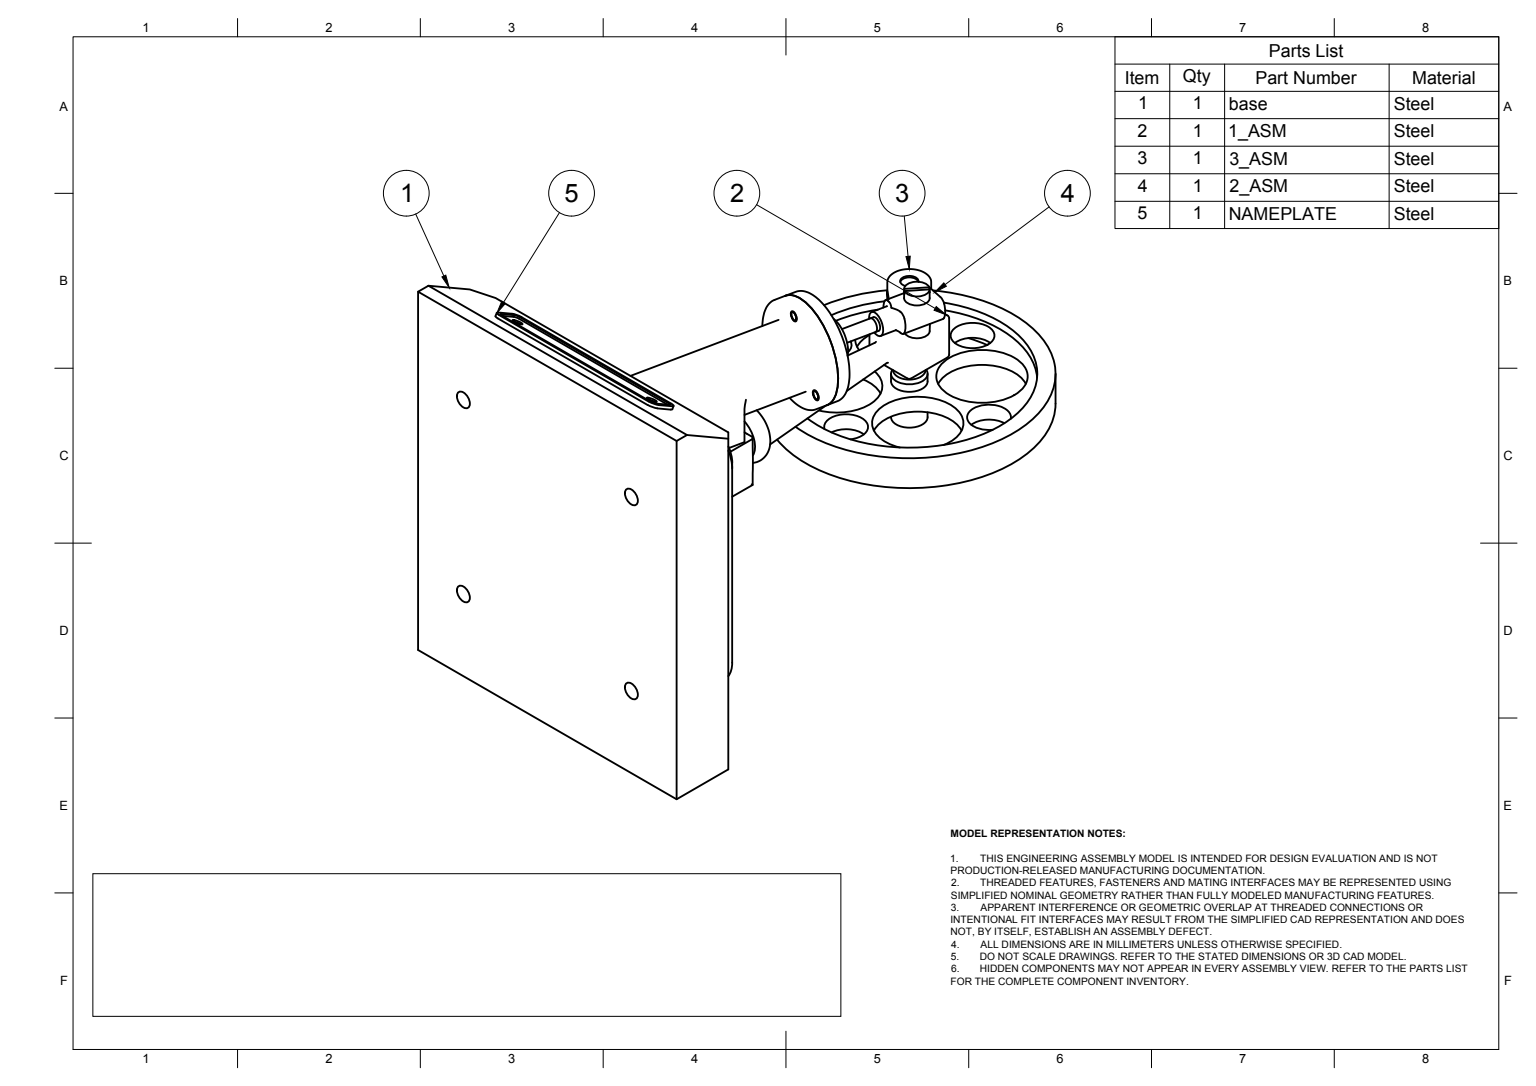
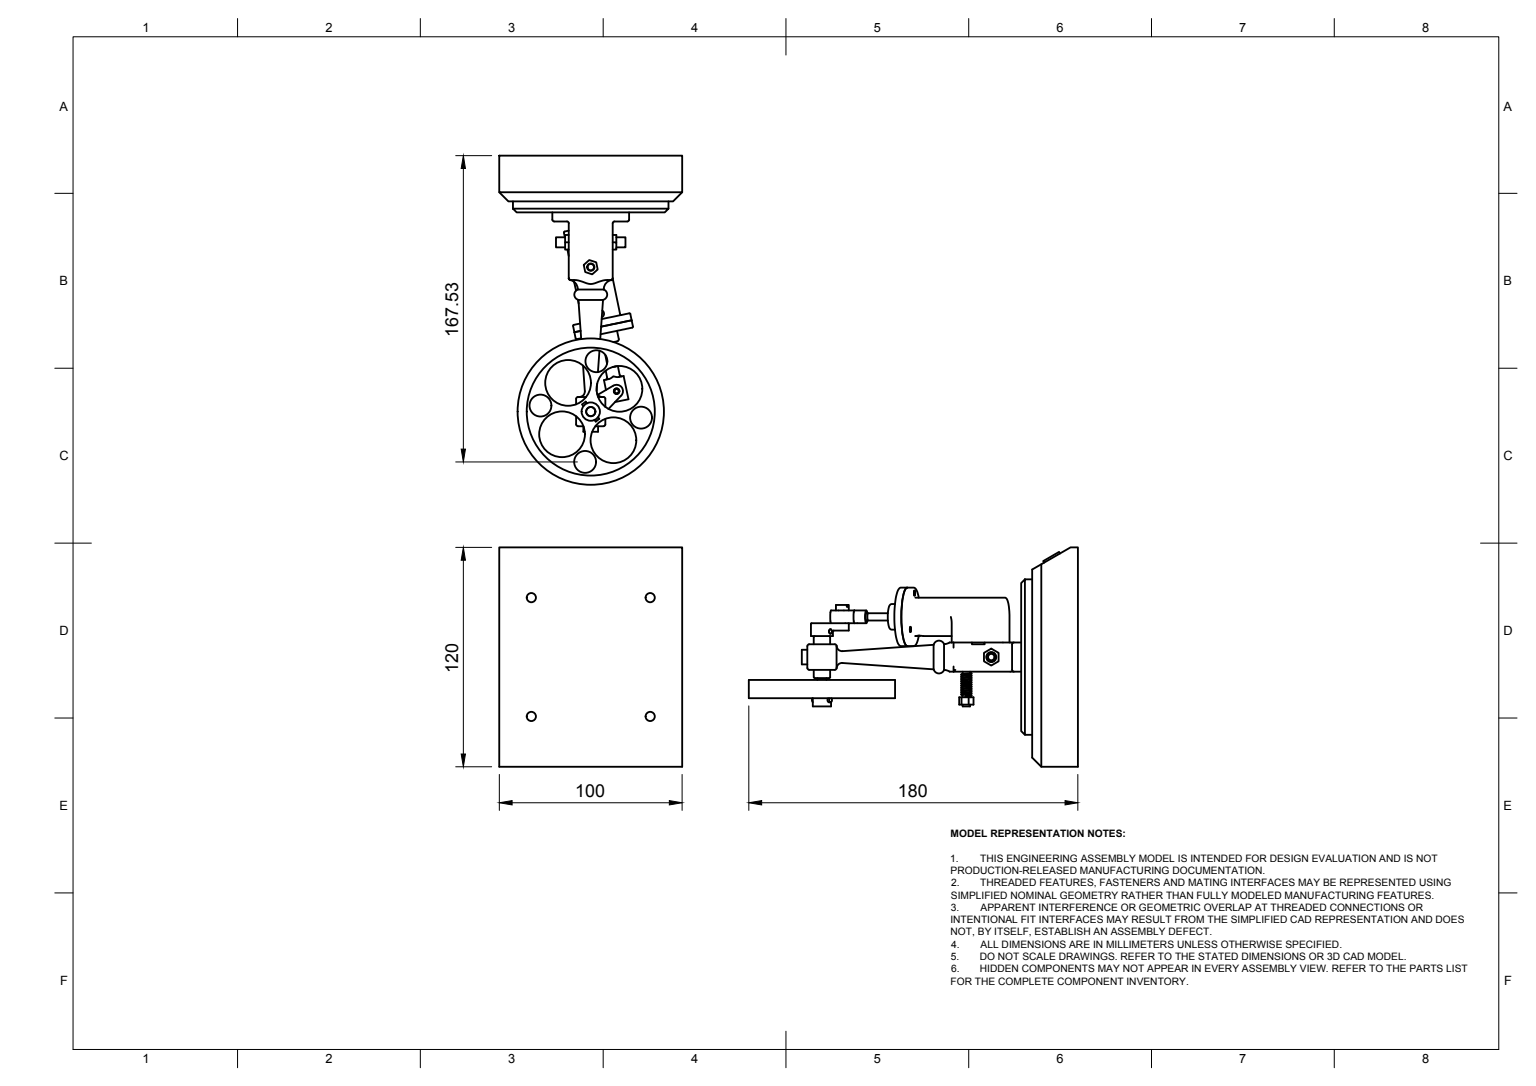
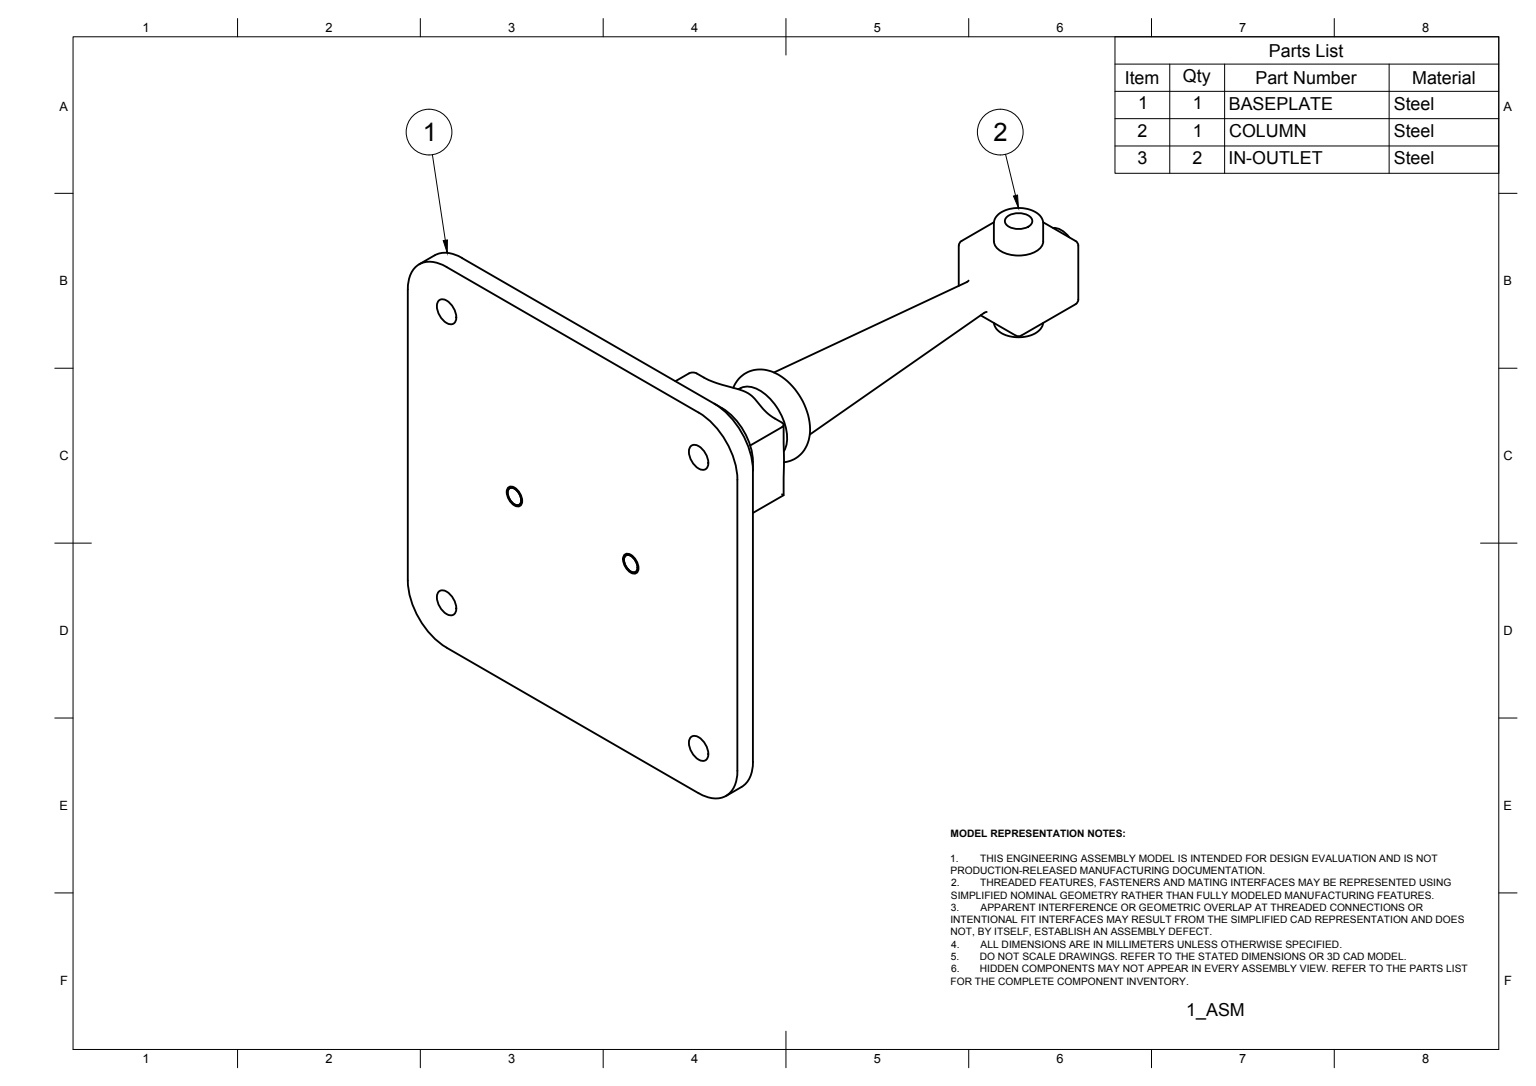
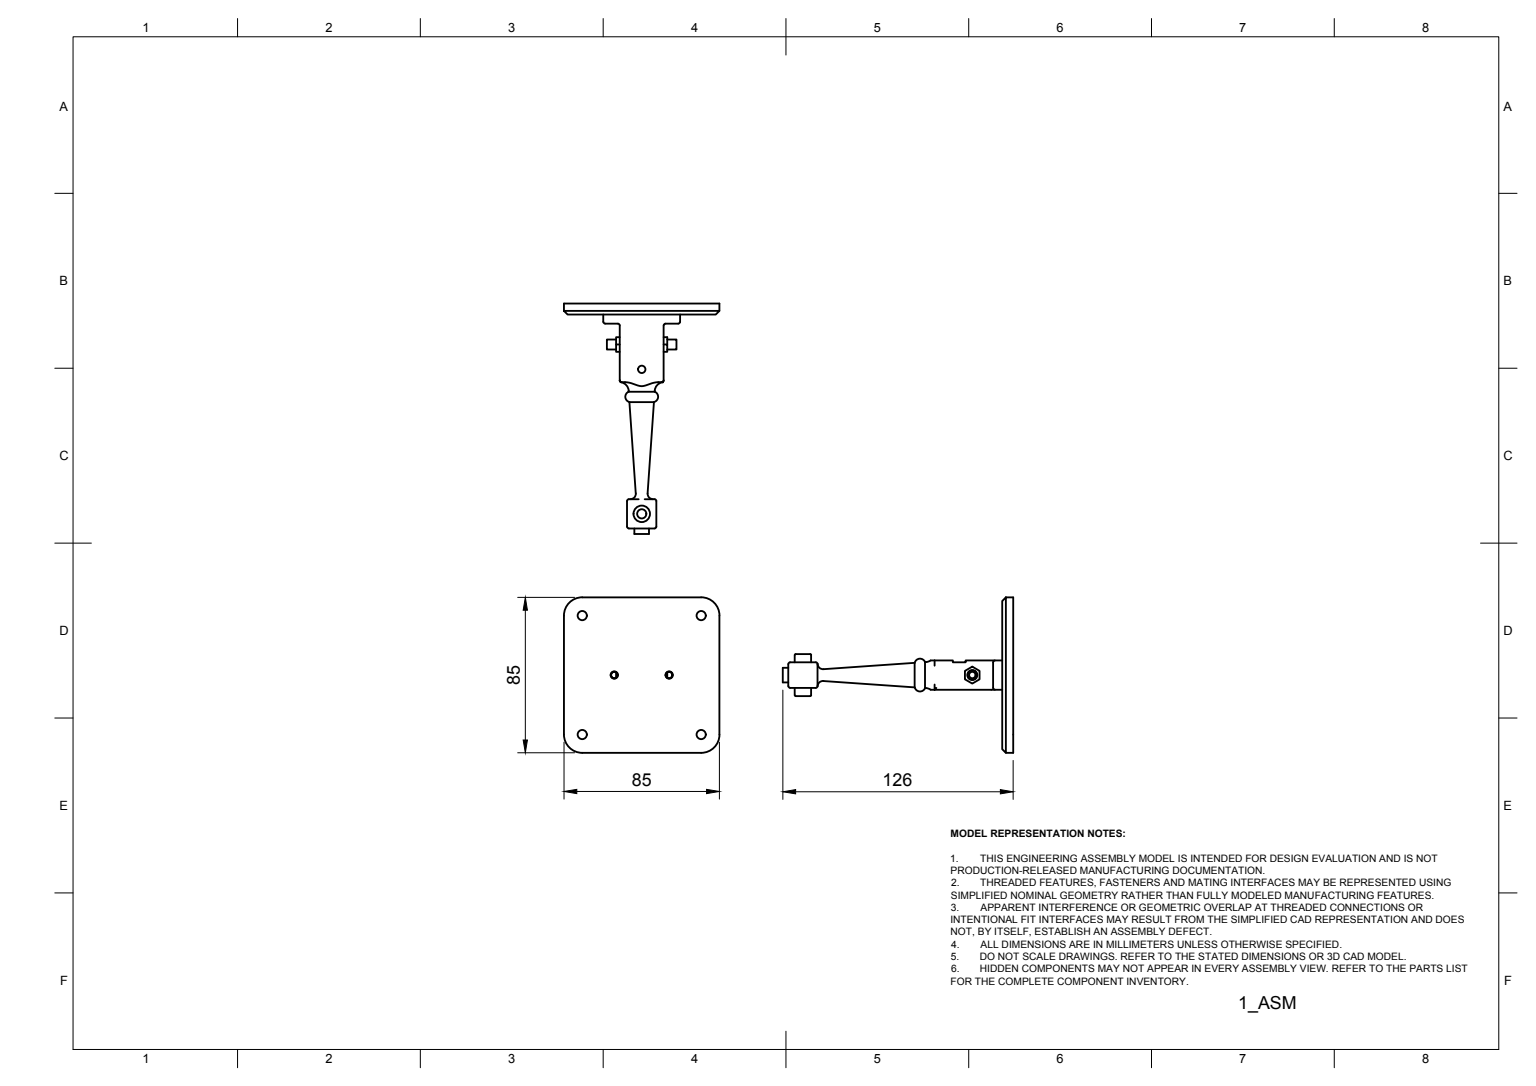
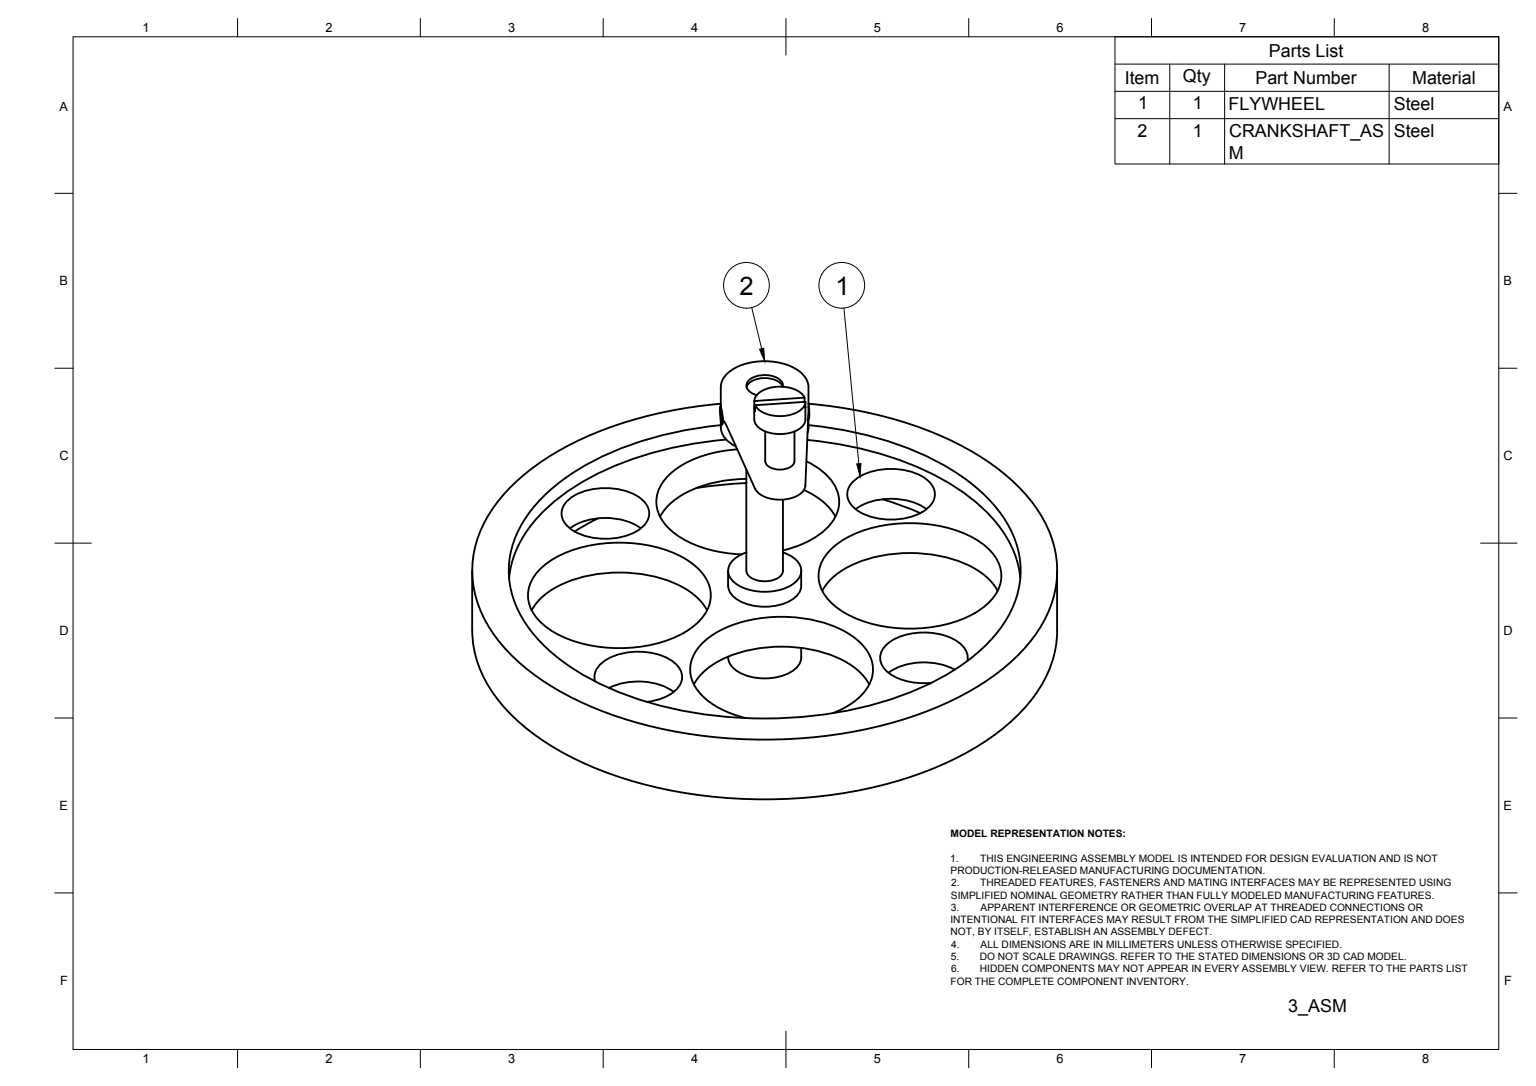
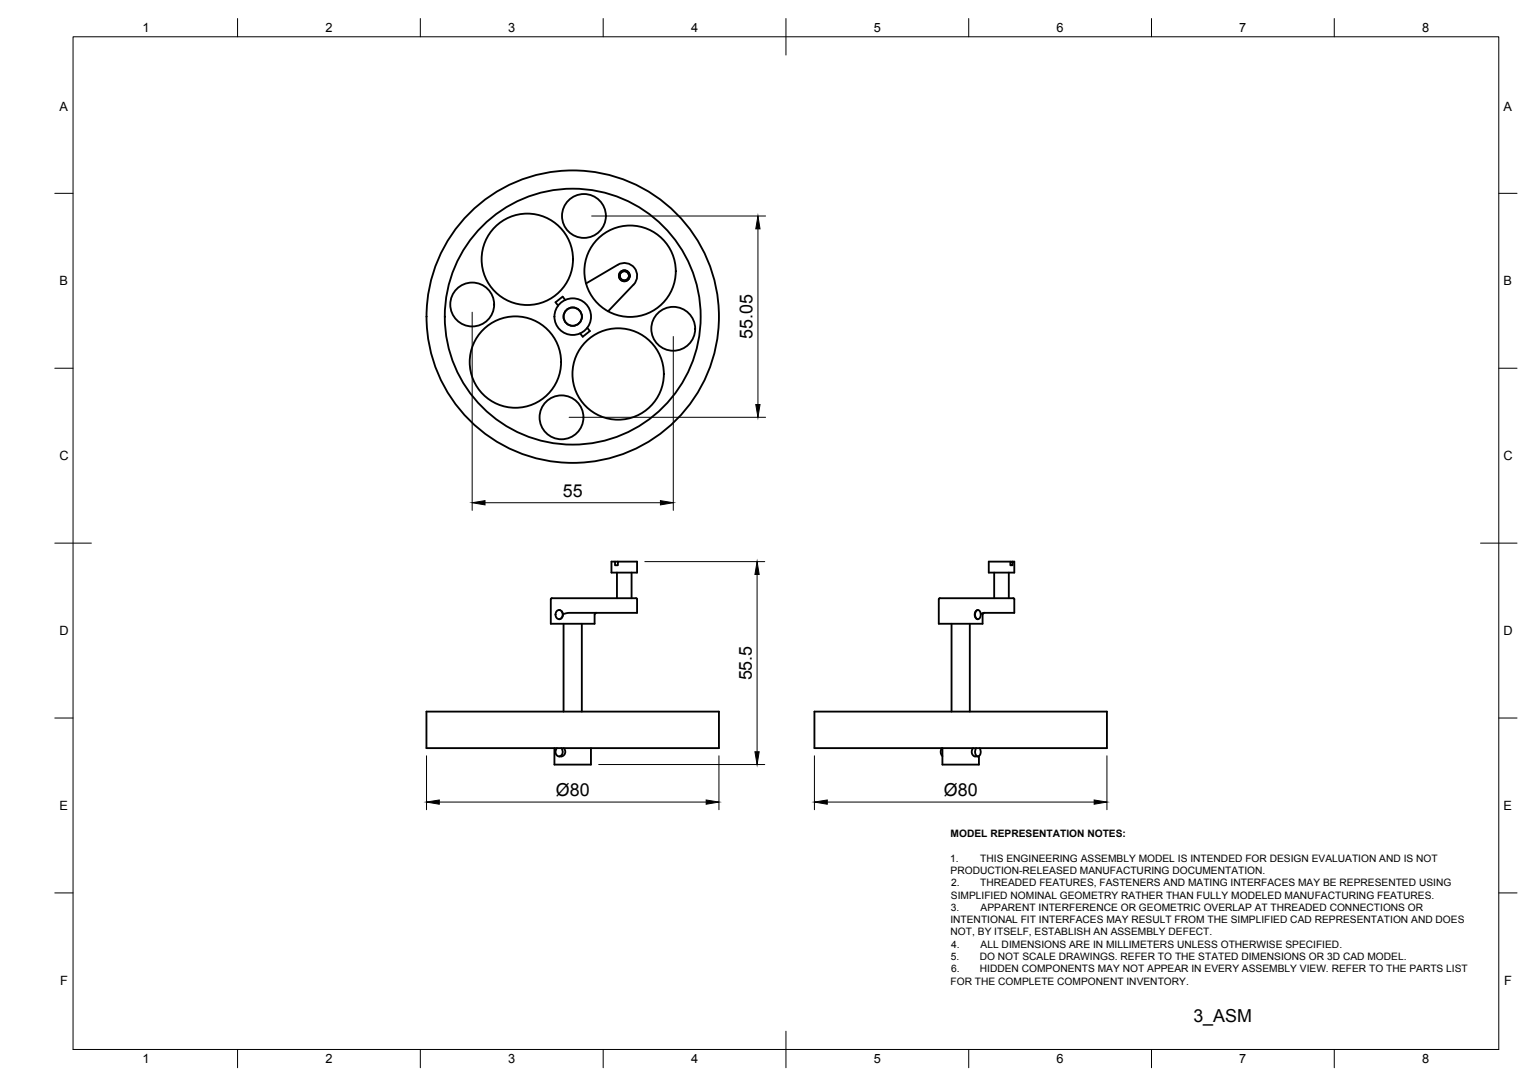
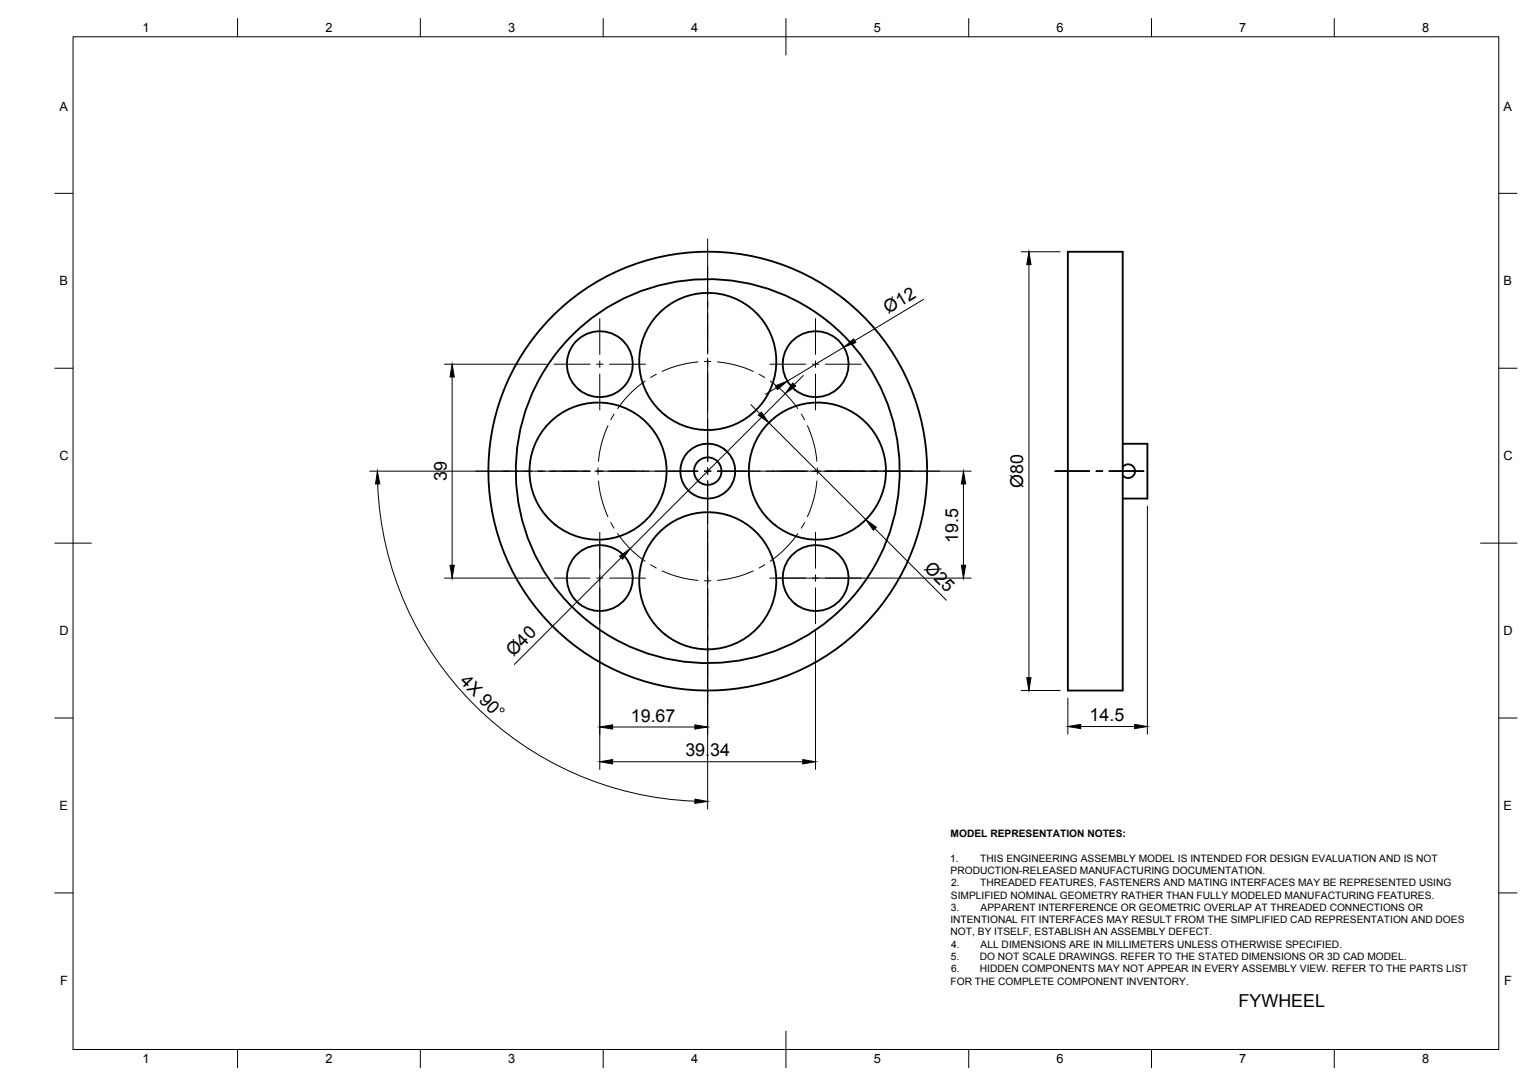
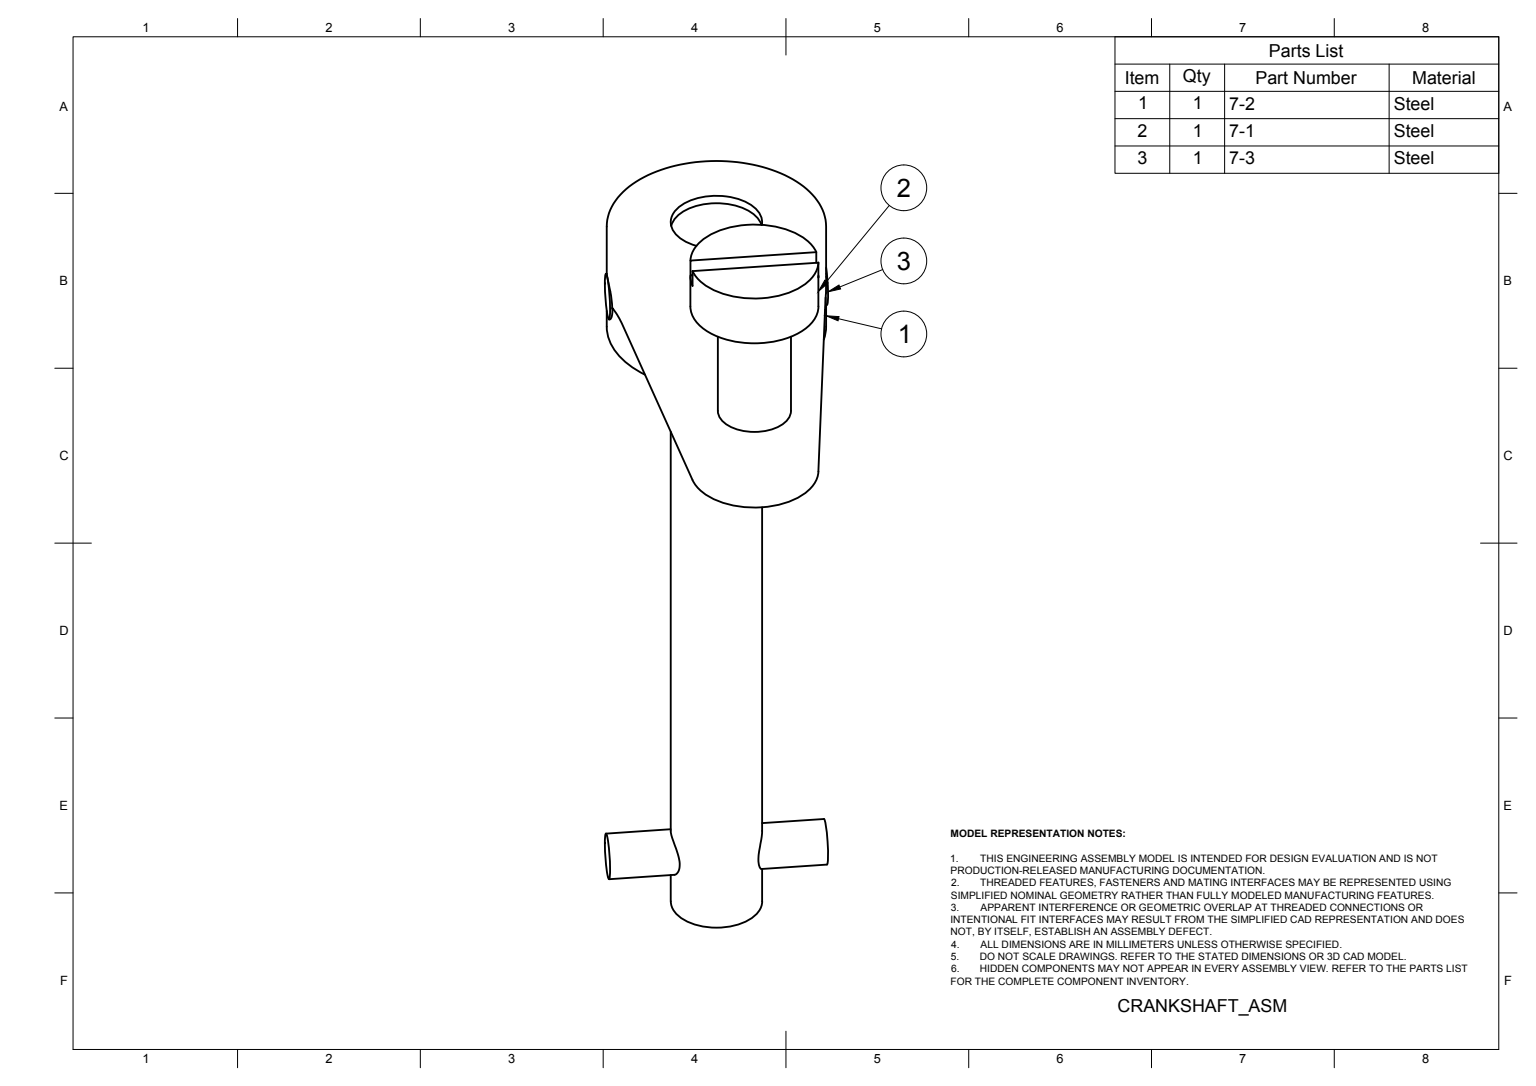
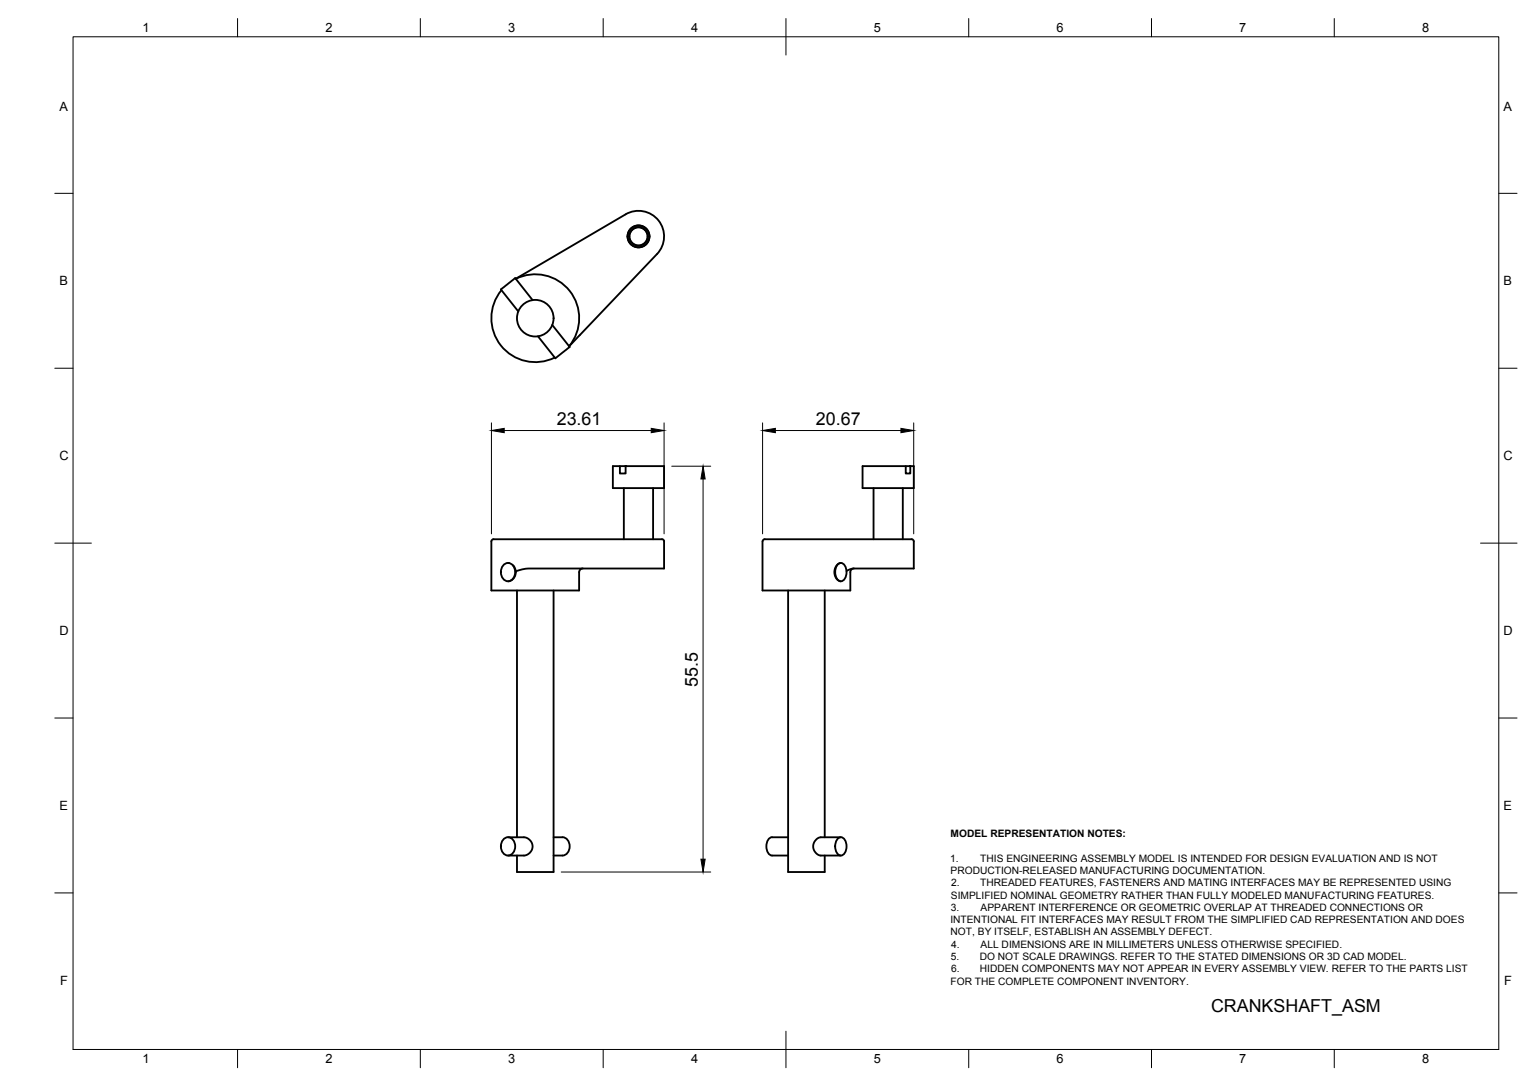
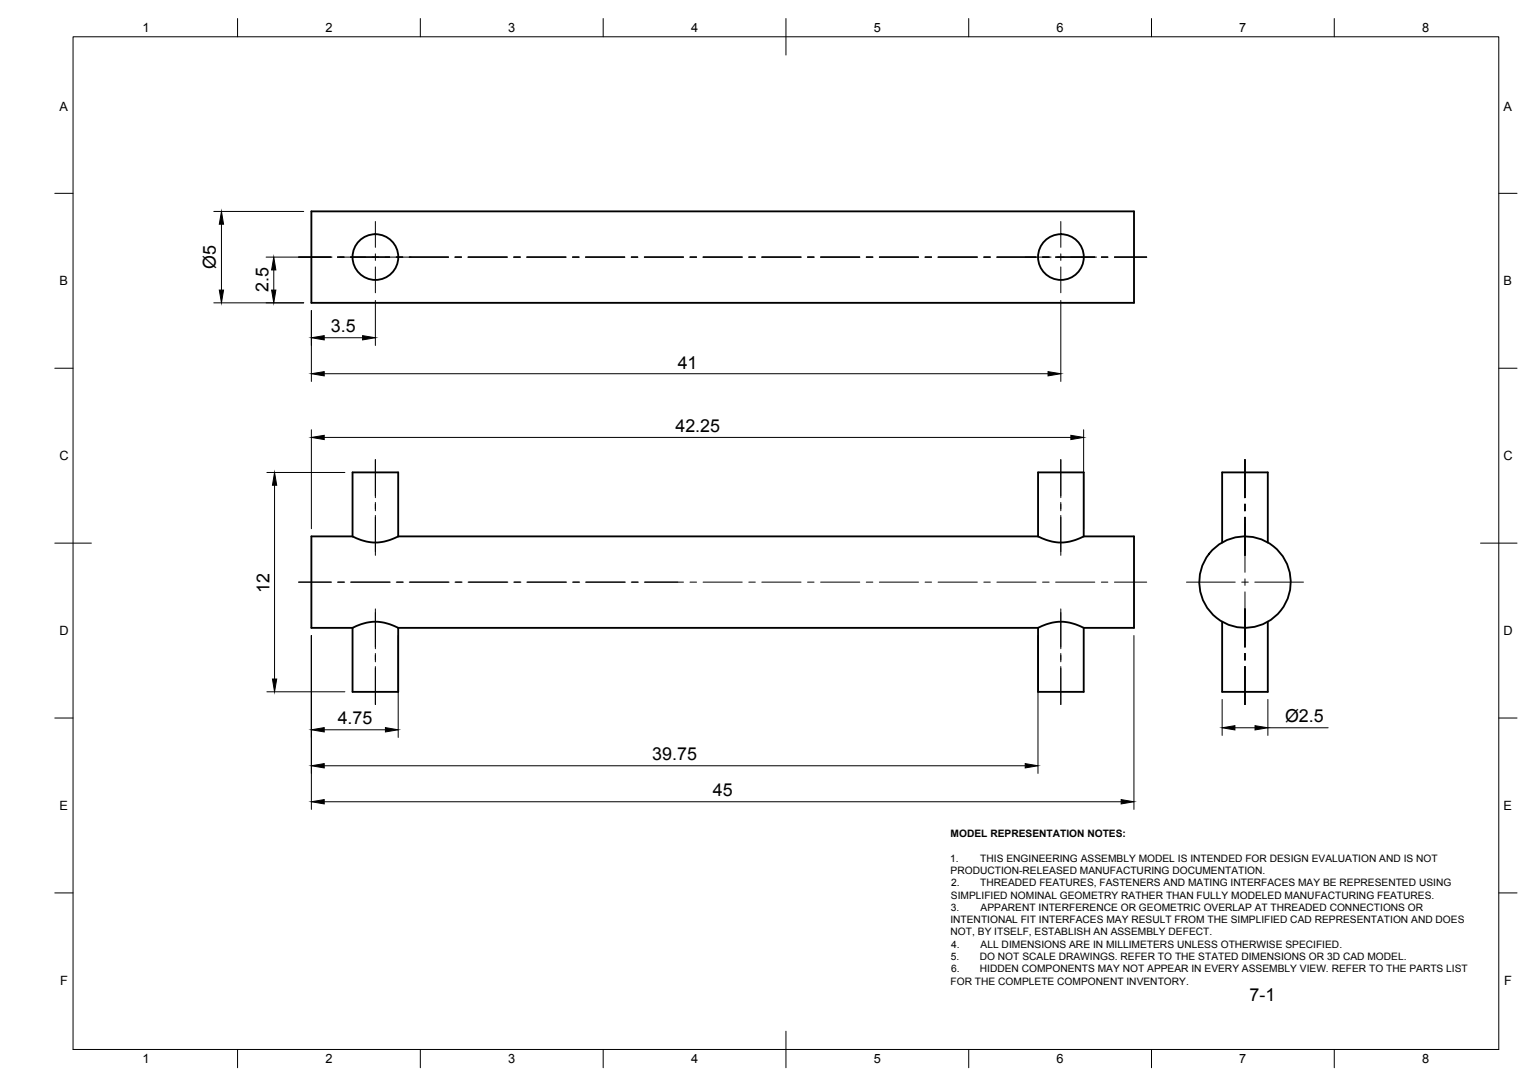
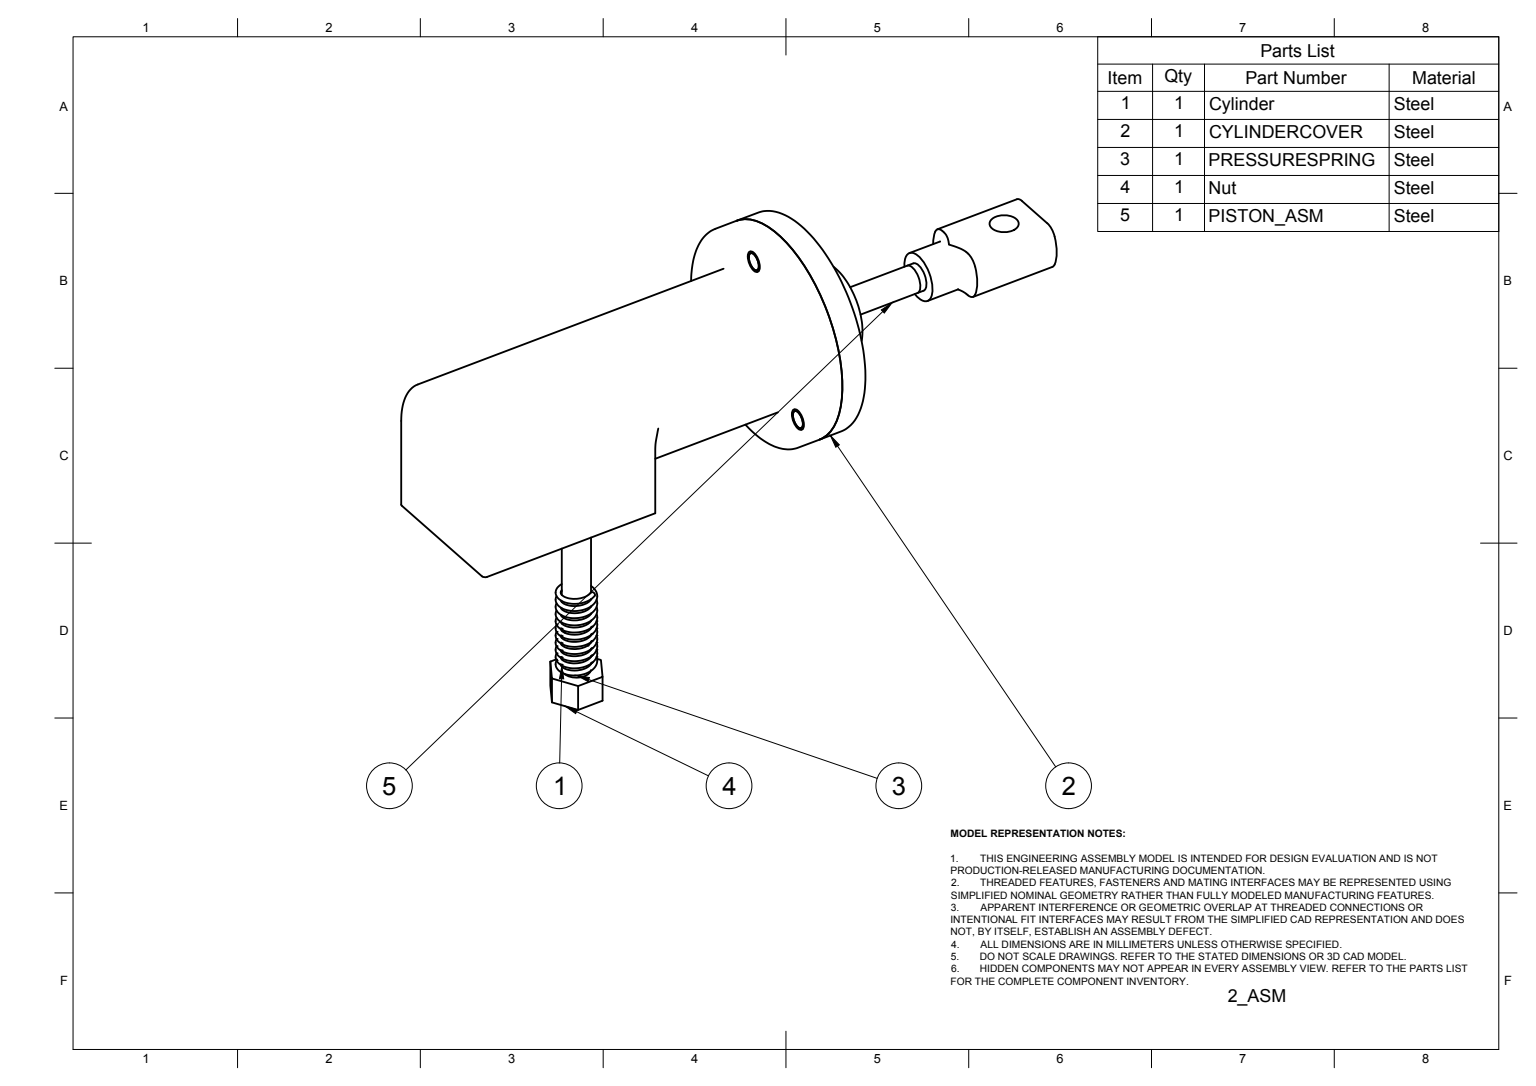
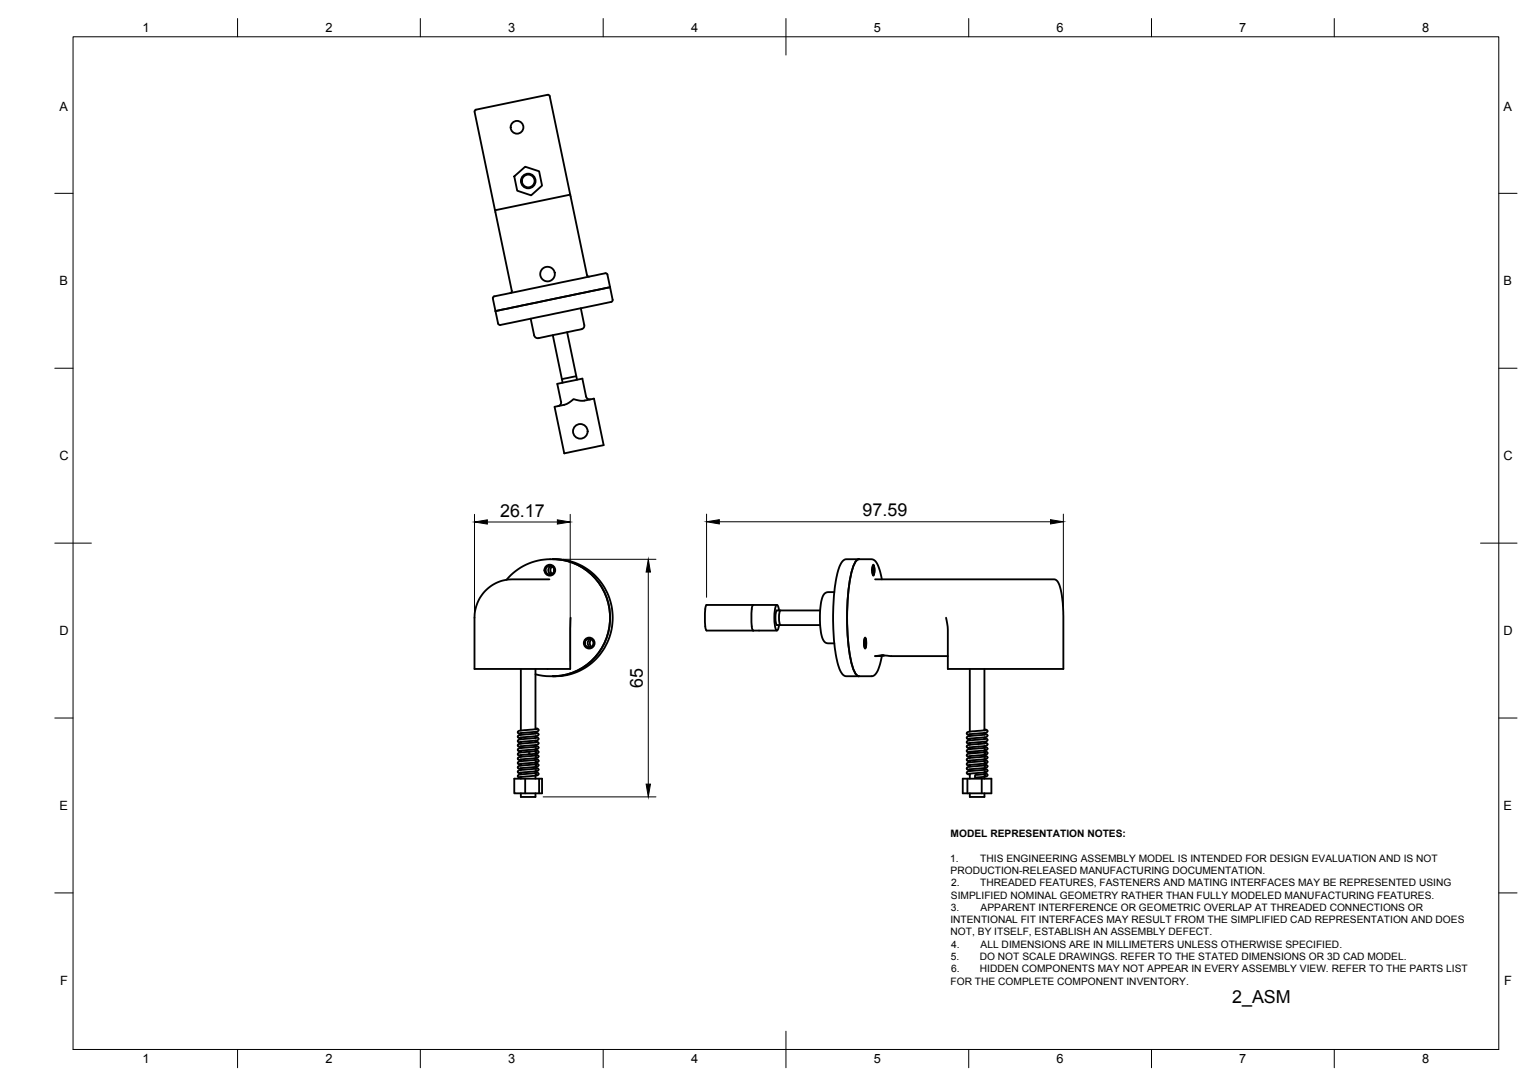
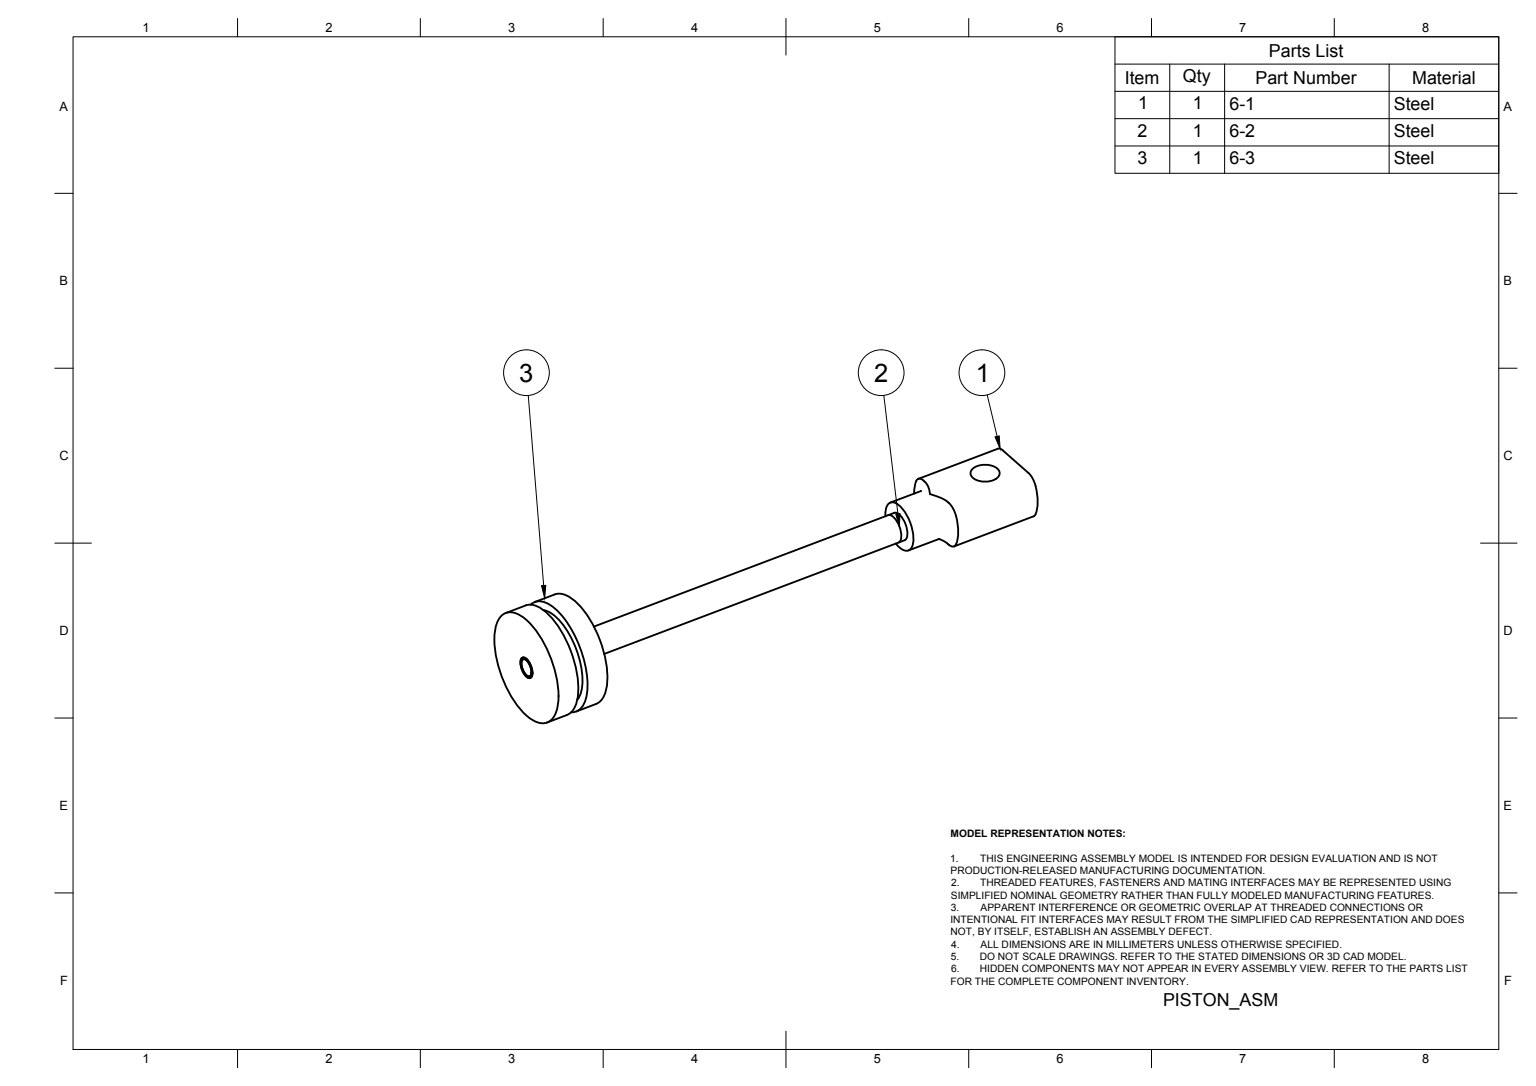
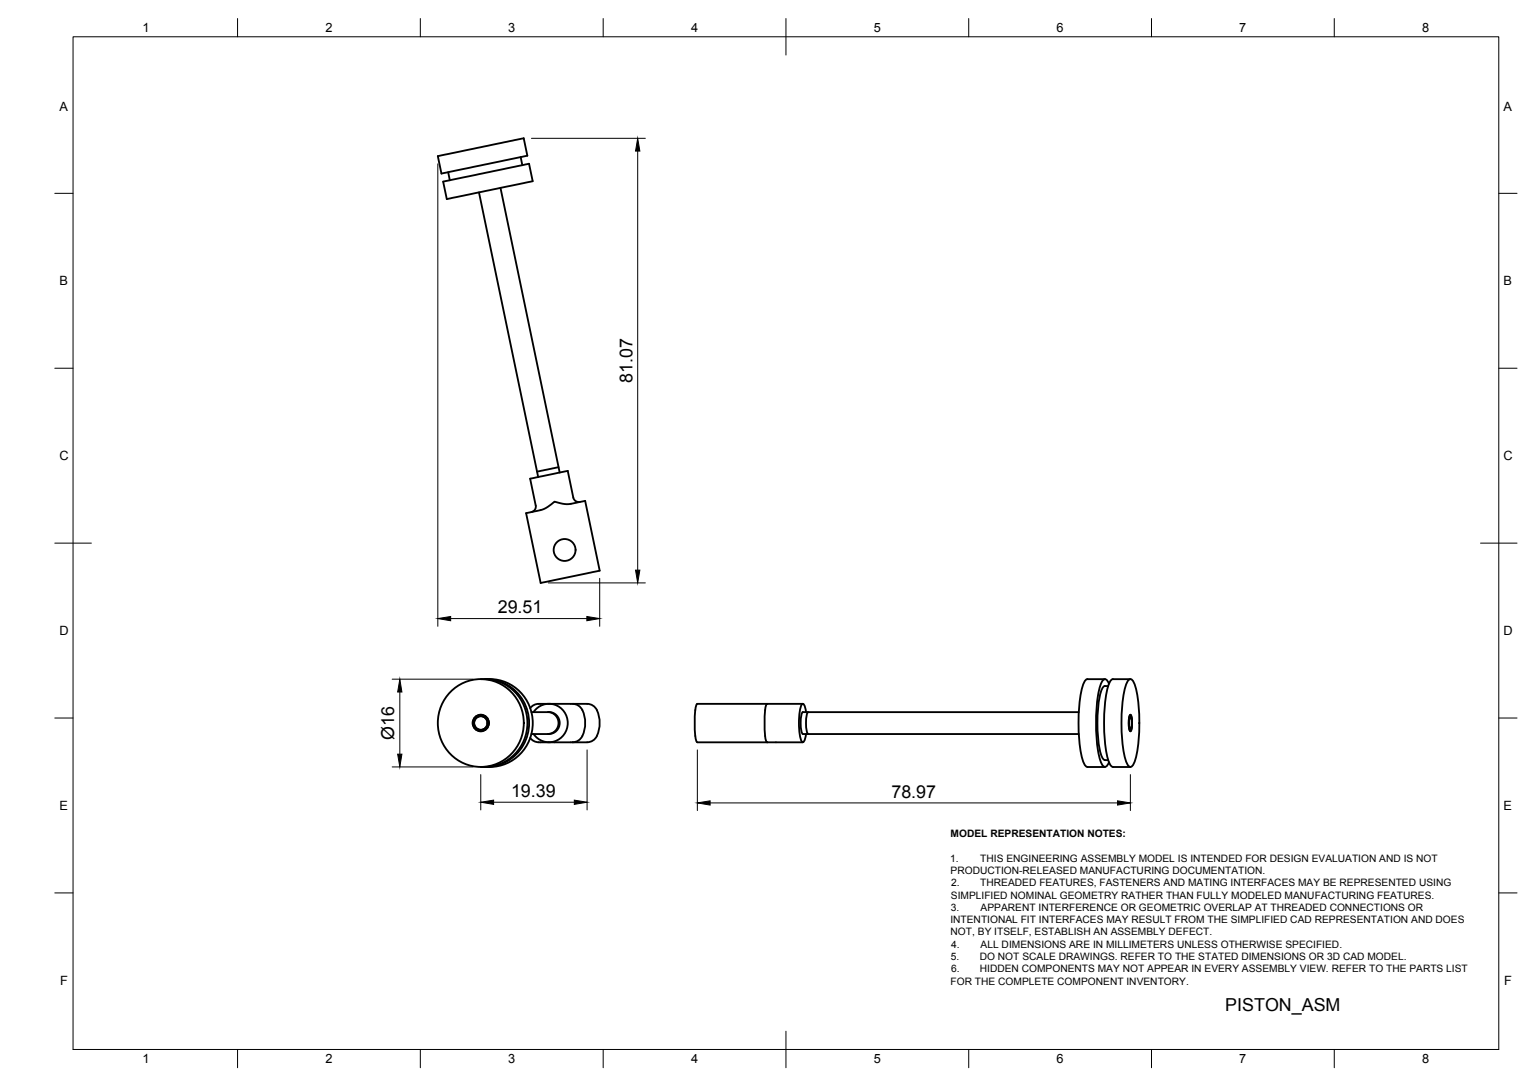
ISO-10303-21;
HEADER;
/* Generated by software containing ST-Developer
 * from STEP Tools, Inc. (www.steptools.com) 
 */

FILE_DESCRIPTION(
/* description */ (''),
/* implementation_level */ '2;1');

FILE_NAME(
/* name */ 'MAS-613',
/* time_stamp */ '2026-10-06T01:16:10-07:00',
/* author */ (''),
/* organization */ (''),
/* preprocessor_version */ 'ST-DEVELOPER v20.2',
/* originating_system */ 'Autodesk Translation Framework v15.15.0.0',
/* authorisation */ '');

FILE_SCHEMA (('AUTOMOTIVE_DESIGN { 1 0 10303 214 3 1 1 }'));
ENDSEC;

DATA;
#10=MECHANICAL_DESIGN_GEOMETRIC_PRESENTATION_REPRESENTATION('',(#296,#297,
#298,#299,#300,#301,#302,#303,#304,#305,#306,#307,#308,#309,#310,#311,#312,
#313,#314,#315,#316,#317,#318,#319,#320,#321,#322,#323,#324,#325,#326,#327,
#328,#329),#17113);
#11=B_SPLINE_SURFACE_WITH_KNOTS('',3,3,((#11570,#11571,#11572,#11573,#11574,
#11575,#11576,#11577,#11578,#11579,#11580,#11581,#11582,#11583,#11584,#11585,
#11586,#11587,#11588,#11589,#11590,#11591,#11592,#11593,#11594,#11595,#11596,
#11597,#11598,#11599,#11600,#11601,#11602,#11603,#11604),(#11605,#11606,
#11607,#11608,#11609,#11610,#11611,#11612,#11613,#11614,#11615,#11616,#11617,
#11618,#11619,#11620,#11621,#11622,#11623,#11624,#11625,#11626,#11627,#11628,
#11629,#11630,#11631,#11632,#11633,#11634,#11635,#11636,#11637,#11638,#11639),
(#11640,#11641,#11642,#11643,#11644,#11645,#11646,#11647,#11648,#11649,
#11650,#11651,#11652,#11653,#11654,#11655,#11656,#11657,#11658,#11659,#11660,
#11661,#11662,#11663,#11664,#11665,#11666,#11667,#11668,#11669,#11670,#11671,
#11672,#11673,#11674),(#11675,#11676,#11677,#11678,#11679,#11680,#11681,
#11682,#11683,#11684,#11685,#11686,#11687,#11688,#11689,#11690,#11691,#11692,
#11693,#11694,#11695,#11696,#11697,#11698,#11699,#11700,#11701,#11702,#11703,
#11704,#11705,#11706,#11707,#11708,#11709),(#11710,#11711,#11712,#11713,
#11714,#11715,#11716,#11717,#11718,#11719,#11720,#11721,#11722,#11723,#11724,
#11725,#11726,#11727,#11728,#11729,#11730,#11731,#11732,#11733,#11734,#11735,
#11736,#11737,#11738,#11739,#11740,#11741,#11742,#11743,#11744),(#11745,
#11746,#11747,#11748,#11749,#11750,#11751,#11752,#11753,#11754,#11755,#11756,
#11757,#11758,#11759,#11760,#11761,#11762,#11763,#11764,#11765,#11766,#11767,
#11768,#11769,#11770,#11771,#11772,#11773,#11774,#11775,#11776,#11777,#11778,
#11779),(#11780,#11781,#11782,#11783,#11784,#11785,#11786,#11787,#11788,
#11789,#11790,#11791,#11792,#11793,#11794,#11795,#11796,#11797,#11798,#11799,
#11800,#11801,#11802,#11803,#11804,#11805,#11806,#11807,#11808,#11809,#11810,
#11811,#11812,#11813,#11814),(#11815,#11816,#11817,#11818,#11819,#11820,
#11821,#11822,#11823,#11824,#11825,#11826,#11827,#11828,#11829,#11830,#11831,
#11832,#11833,#11834,#11835,#11836,#11837,#11838,#11839,#11840,#11841,#11842,
#11843,#11844,#11845,#11846,#11847,#11848,#11849),(#11850,#11851,#11852,
#11853,#11854,#11855,#11856,#11857,#11858,#11859,#11860,#11861,#11862,#11863,
#11864,#11865,#11866,#11867,#11868,#11869,#11870,#11871,#11872,#11873,#11874,
#11875,#11876,#11877,#11878,#11879,#11880,#11881,#11882,#11883,#11884),
(#11885,#11886,#11887,#11888,#11889,#11890,#11891,#11892,#11893,#11894,
#11895,#11896,#11897,#11898,#11899,#11900,#11901,#11902,#11903,#11904,#11905,
#11906,#11907,#11908,#11909,#11910,#11911,#11912,#11913,#11914,#11915,#11916,
#11917,#11918,#11919)),.UNSPECIFIED.,.F.,.F.,.F.,(4,1,1,1,1,1,1,4),(4,1,
1,1,1,1,1,1,1,1,1,1,1,1,1,1,1,1,1,1,1,1,1,1,1,1,1,1,1,1,1,1,4),(-0.05714514294858,
0.,0.125,0.25,0.3267862857371,0.4035725714743,0.4803588572114,0.5571451429486),
(-0.02,0.0125,0.045,0.0775,0.11,0.1425,0.175,0.2075,0.24,0.2725,0.305,0.3375,
0.37,0.4025,0.435,0.4675,0.5,0.5325,0.565,0.5975,0.63,0.6625,0.695,0.7275,
0.76,0.7925,0.825,0.8575,0.89,0.9225,0.955,0.9875,1.02),.UNSPECIFIED.);
#12=B_SPLINE_SURFACE_WITH_KNOTS('',3,3,((#13047,#13048,#13049,#13050,#13051,
#13052,#13053,#13054,#13055,#13056,#13057,#13058,#13059,#13060,#13061,#13062,
#13063,#13064,#13065,#13066,#13067,#13068,#13069,#13070,#13071,#13072,#13073,
#13074,#13075,#13076,#13077,#13078,#13079,#13080,#13081),(#13082,#13083,
#13084,#13085,#13086,#13087,#13088,#13089,#13090,#13091,#13092,#13093,#13094,
#13095,#13096,#13097,#13098,#13099,#13100,#13101,#13102,#13103,#13104,#13105,
#13106,#13107,#13108,#13109,#13110,#13111,#13112,#13113,#13114,#13115,#13116),
(#13117,#13118,#13119,#13120,#13121,#13122,#13123,#13124,#13125,#13126,
#13127,#13128,#13129,#13130,#13131,#13132,#13133,#13134,#13135,#13136,#13137,
#13138,#13139,#13140,#13141,#13142,#13143,#13144,#13145,#13146,#13147,#13148,
#13149,#13150,#13151),(#13152,#13153,#13154,#13155,#13156,#13157,#13158,
#13159,#13160,#13161,#13162,#13163,#13164,#13165,#13166,#13167,#13168,#13169,
#13170,#13171,#13172,#13173,#13174,#13175,#13176,#13177,#13178,#13179,#13180,
#13181,#13182,#13183,#13184,#13185,#13186),(#13187,#13188,#13189,#13190,
#13191,#13192,#13193,#13194,#13195,#13196,#13197,#13198,#13199,#13200,#13201,
#13202,#13203,#13204,#13205,#13206,#13207,#13208,#13209,#13210,#13211,#13212,
#13213,#13214,#13215,#13216,#13217,#13218,#13219,#13220,#13221),(#13222,
#13223,#13224,#13225,#13226,#13227,#13228,#13229,#13230,#13231,#13232,#13233,
#13234,#13235,#13236,#13237,#13238,#13239,#13240,#13241,#13242,#13243,#13244,
#13245,#13246,#13247,#13248,#13249,#13250,#13251,#13252,#13253,#13254,#13255,
#13256),(#13257,#13258,#13259,#13260,#13261,#13262,#13263,#13264,#13265,
#13266,#13267,#13268,#13269,#13270,#13271,#13272,#13273,#13274,#13275,#13276,
#13277,#13278,#13279,#13280,#13281,#13282,#13283,#13284,#13285,#13286,#13287,
#13288,#13289,#13290,#13291)),.UNSPECIFIED.,.F.,.F.,.F.,(4,1,1,1,4),(4,
1,1,1,1,1,1,1,1,1,1,1,1,1,1,1,1,1,1,1,1,1,1,1,1,1,1,1,1,1,1,1,4),(0.4428548570514,
0.5,0.75,1.,1.057145142949),(-0.02,0.0125,0.045,0.0775,0.11,0.1425,0.175,
0.2075,0.24,0.2725,0.305,0.3375,0.37,0.4025,0.435,0.4675,0.5,0.5325,0.565,
0.5975,0.63,0.6625,0.695,0.7275,0.76,0.7925,0.825,0.8575,0.89,0.9225,0.955,
0.9875,1.02),.UNSPECIFIED.);
#13=B_SPLINE_SURFACE_WITH_KNOTS('',3,3,((#13335,#13336,#13337,#13338,#13339,
#13340,#13341,#13342,#13343,#13344,#13345,#13346,#13347,#13348,#13349,#13350,
#13351,#13352,#13353,#13354,#13355,#13356,#13357,#13358,#13359,#13360,#13361,
#13362,#13363,#13364,#13365,#13366,#13367,#13368,#13369),(#13370,#13371,
#13372,#13373,#13374,#13375,#13376,#13377,#13378,#13379,#13380,#13381,#13382,
#13383,#13384,#13385,#13386,#13387,#13388,#13389,#13390,#13391,#13392,#13393,
#13394,#13395,#13396,#13397,#13398,#13399,#13400,#13401,#13402,#13403,#13404),
(#13405,#13406,#13407,#13408,#13409,#13410,#13411,#13412,#13413,#13414,
#13415,#13416,#13417,#13418,#13419,#13420,#13421,#13422,#13423,#13424,#13425,
#13426,#13427,#13428,#13429,#13430,#13431,#13432,#13433,#13434,#13435,#13436,
#13437,#13438,#13439),(#13440,#13441,#13442,#13443,#13444,#13445,#13446,
#13447,#13448,#13449,#13450,#13451,#13452,#13453,#13454,#13455,#13456,#13457,
#13458,#13459,#13460,#13461,#13462,#13463,#13464,#13465,#13466,#13467,#13468,
#13469,#13470,#13471,#13472,#13473,#13474),(#13475,#13476,#13477,#13478,
#13479,#13480,#13481,#13482,#13483,#13484,#13485,#13486,#13487,#13488,#13489,
#13490,#13491,#13492,#13493,#13494,#13495,#13496,#13497,#13498,#13499,#13500,
#13501,#13502,#13503,#13504,#13505,#13506,#13507,#13508,#13509),(#13510,
#13511,#13512,#13513,#13514,#13515,#13516,#13517,#13518,#13519,#13520,#13521,
#13522,#13523,#13524,#13525,#13526,#13527,#13528,#13529,#13530,#13531,#13532,
#13533,#13534,#13535,#13536,#13537,#13538,#13539,#13540,#13541,#13542,#13543,
#13544),(#13545,#13546,#13547,#13548,#13549,#13550,#13551,#13552,#13553,
#13554,#13555,#13556,#13557,#13558,#13559,#13560,#13561,#13562,#13563,#13564,
#13565,#13566,#13567,#13568,#13569,#13570,#13571,#13572,#13573,#13574,#13575,
#13576,#13577,#13578,#13579)),.UNSPECIFIED.,.F.,.F.,.F.,(4,1,1,1,4),(4,
1,1,1,1,1,1,1,1,1,1,1,1,1,1,1,1,1,1,1,1,1,1,1,1,1,1,1,1,1,1,1,4),(0.4428548570514,
0.5,0.75,1.,1.057145142949),(-0.02,0.0125,0.045,0.0775,0.11,0.1425,0.175,
0.2075,0.24,0.2725,0.305,0.3375,0.37,0.4025,0.435,0.4675,0.5,0.5325,0.565,
0.5975,0.63,0.6625,0.695,0.7275,0.76,0.7925,0.825,0.8575,0.89,0.9225,0.955,
0.9875,1.02),.UNSPECIFIED.);
#14=B_SPLINE_SURFACE_WITH_KNOTS('',3,3,((#14695,#14696,#14697,#14698,#14699,
#14700,#14701,#14702,#14703,#14704,#14705,#14706,#14707,#14708,#14709,#14710,
#14711,#14712,#14713,#14714,#14715,#14716,#14717,#14718,#14719,#14720,#14721,
#14722,#14723,#14724,#14725,#14726,#14727,#14728,#14729),(#14730,#14731,
#14732,#14733,#14734,#14735,#14736,#14737,#14738,#14739,#14740,#14741,#14742,
#14743,#14744,#14745,#14746,#14747,#14748,#14749,#14750,#14751,#14752,#14753,
#14754,#14755,#14756,#14757,#14758,#14759,#14760,#14761,#14762,#14763,#14764),
(#14765,#14766,#14767,#14768,#14769,#14770,#14771,#14772,#14773,#14774,
#14775,#14776,#14777,#14778,#14779,#14780,#14781,#14782,#14783,#14784,#14785,
#14786,#14787,#14788,#14789,#14790,#14791,#14792,#14793,#14794,#14795,#14796,
#14797,#14798,#14799),(#14800,#14801,#14802,#14803,#14804,#14805,#14806,
#14807,#14808,#14809,#14810,#14811,#14812,#14813,#14814,#14815,#14816,#14817,
#14818,#14819,#14820,#14821,#14822,#14823,#14824,#14825,#14826,#14827,#14828,
#14829,#14830,#14831,#14832,#14833,#14834),(#14835,#14836,#14837,#14838,
#14839,#14840,#14841,#14842,#14843,#14844,#14845,#14846,#14847,#14848,#14849,
#14850,#14851,#14852,#14853,#14854,#14855,#14856,#14857,#14858,#14859,#14860,
#14861,#14862,#14863,#14864,#14865,#14866,#14867,#14868,#14869),(#14870,
#14871,#14872,#14873,#14874,#14875,#14876,#14877,#14878,#14879,#14880,#14881,
#14882,#14883,#14884,#14885,#14886,#14887,#14888,#14889,#14890,#14891,#14892,
#14893,#14894,#14895,#14896,#14897,#14898,#14899,#14900,#14901,#14902,#14903,
#14904),(#14905,#14906,#14907,#14908,#14909,#14910,#14911,#14912,#14913,
#14914,#14915,#14916,#14917,#14918,#14919,#14920,#14921,#14922,#14923,#14924,
#14925,#14926,#14927,#14928,#14929,#14930,#14931,#14932,#14933,#14934,#14935,
#14936,#14937,#14938,#14939),(#14940,#14941,#14942,#14943,#14944,#14945,
#14946,#14947,#14948,#14949,#14950,#14951,#14952,#14953,#14954,#14955,#14956,
#14957,#14958,#14959,#14960,#14961,#14962,#14963,#14964,#14965,#14966,#14967,
#14968,#14969,#14970,#14971,#14972,#14973,#14974),(#14975,#14976,#14977,
#14978,#14979,#14980,#14981,#14982,#14983,#14984,#14985,#14986,#14987,#14988,
#14989,#14990,#14991,#14992,#14993,#14994,#14995,#14996,#14997,#14998,#14999,
#15000,#15001,#15002,#15003,#15004,#15005,#15006,#15007,#15008,#15009),
(#15010,#15011,#15012,#15013,#15014,#15015,#15016,#15017,#15018,#15019,
#15020,#15021,#15022,#15023,#15024,#15025,#15026,#15027,#15028,#15029,#15030,
#15031,#15032,#15033,#15034,#15035,#15036,#15037,#15038,#15039,#15040,#15041,
#15042,#15043,#15044)),.UNSPECIFIED.,.F.,.F.,.F.,(4,1,1,1,1,1,1,4),(4,1,
1,1,1,1,1,1,1,1,1,1,1,1,1,1,1,1,1,1,1,1,1,1,1,1,1,1,1,1,1,1,4),(-0.05714514294857,
0.,0.125,0.25,0.3267862857371,0.4035725714743,0.4803588572114,0.5571451429486),
(-0.02,0.0125,0.045,0.0775,0.11,0.1425,0.175,0.2075,0.24,0.2725,0.305,0.3375,
0.37,0.4025,0.435,0.4675,0.5,0.5325,0.565,0.5975,0.63,0.6625,0.695,0.7275,
0.76,0.7925,0.825,0.8575,0.89,0.9225,0.955,0.9875,1.02),.UNSPECIFIED.);
#15=B_SPLINE_SURFACE_WITH_KNOTS('',3,3,((#15100,#15101,#15102,#15103,#15104,
#15105,#15106,#15107,#15108,#15109,#15110,#15111,#15112,#15113,#15114,#15115,
#15116,#15117,#15118,#15119,#15120,#15121,#15122,#15123,#15124,#15125,#15126,
#15127,#15128,#15129,#15130,#15131,#15132,#15133,#15134),(#15135,#15136,
#15137,#15138,#15139,#15140,#15141,#15142,#15143,#15144,#15145,#15146,#15147,
#15148,#15149,#15150,#15151,#15152,#15153,#15154,#15155,#15156,#15157,#15158,
#15159,#15160,#15161,#15162,#15163,#15164,#15165,#15166,#15167,#15168,#15169),
(#15170,#15171,#15172,#15173,#15174,#15175,#15176,#15177,#15178,#15179,
#15180,#15181,#15182,#15183,#15184,#15185,#15186,#15187,#15188,#15189,#15190,
#15191,#15192,#15193,#15194,#15195,#15196,#15197,#15198,#15199,#15200,#15201,
#15202,#15203,#15204),(#15205,#15206,#15207,#15208,#15209,#15210,#15211,
#15212,#15213,#15214,#15215,#15216,#15217,#15218,#15219,#15220,#15221,#15222,
#15223,#15224,#15225,#15226,#15227,#15228,#15229,#15230,#15231,#15232,#15233,
#15234,#15235,#15236,#15237,#15238,#15239),(#15240,#15241,#15242,#15243,
#15244,#15245,#15246,#15247,#15248,#15249,#15250,#15251,#15252,#15253,#15254,
#15255,#15256,#15257,#15258,#15259,#15260,#15261,#15262,#15263,#15264,#15265,
#15266,#15267,#15268,#15269,#15270,#15271,#15272,#15273,#15274),(#15275,
#15276,#15277,#15278,#15279,#15280,#15281,#15282,#15283,#15284,#15285,#15286,
#15287,#15288,#15289,#15290,#15291,#15292,#15293,#15294,#15295,#15296,#15297,
#15298,#15299,#15300,#15301,#15302,#15303,#15304,#15305,#15306,#15307,#15308,
#15309),(#15310,#15311,#15312,#15313,#15314,#15315,#15316,#15317,#15318,
#15319,#15320,#15321,#15322,#15323,#15324,#15325,#15326,#15327,#15328,#15329,
#15330,#15331,#15332,#15333,#15334,#15335,#15336,#15337,#15338,#15339,#15340,
#15341,#15342,#15343,#15344)),.UNSPECIFIED.,.F.,.F.,.F.,(4,1,1,1,4),(4,
1,1,1,1,1,1,1,1,1,1,1,1,1,1,1,1,1,1,1,1,1,1,1,1,1,1,1,1,1,1,1,4),(-0.05714514294858,
0.,0.25,0.5,0.5571451429486),(-0.02,0.0125,0.045,0.0775,0.11,0.1425,0.175,
0.2075,0.24,0.2725,0.305,0.3375,0.37,0.4025,0.435,0.4675,0.5,0.5325,0.565,
0.5975,0.63,0.6625,0.695,0.7275,0.76,0.7925,0.825,0.8575,0.89,0.9225,0.955,
0.9875,1.02),.UNSPECIFIED.);
#16=B_SPLINE_SURFACE_WITH_KNOTS('',3,3,((#16439,#16440,#16441,#16442,#16443,
#16444,#16445,#16446,#16447,#16448,#16449,#16450,#16451,#16452,#16453,#16454,
#16455,#16456,#16457,#16458,#16459,#16460,#16461,#16462,#16463,#16464,#16465,
#16466,#16467,#16468,#16469,#16470,#16471,#16472,#16473),(#16474,#16475,
#16476,#16477,#16478,#16479,#16480,#16481,#16482,#16483,#16484,#16485,#16486,
#16487,#16488,#16489,#16490,#16491,#16492,#16493,#16494,#16495,#16496,#16497,
#16498,#16499,#16500,#16501,#16502,#16503,#16504,#16505,#16506,#16507,#16508),
(#16509,#16510,#16511,#16512,#16513,#16514,#16515,#16516,#16517,#16518,
#16519,#16520,#16521,#16522,#16523,#16524,#16525,#16526,#16527,#16528,#16529,
#16530,#16531,#16532,#16533,#16534,#16535,#16536,#16537,#16538,#16539,#16540,
#16541,#16542,#16543),(#16544,#16545,#16546,#16547,#16548,#16549,#16550,
#16551,#16552,#16553,#16554,#16555,#16556,#16557,#16558,#16559,#16560,#16561,
#16562,#16563,#16564,#16565,#16566,#16567,#16568,#16569,#16570,#16571,#16572,
#16573,#16574,#16575,#16576,#16577,#16578),(#16579,#16580,#16581,#16582,
#16583,#16584,#16585,#16586,#16587,#16588,#16589,#16590,#16591,#16592,#16593,
#16594,#16595,#16596,#16597,#16598,#16599,#16600,#16601,#16602,#16603,#16604,
#16605,#16606,#16607,#16608,#16609,#16610,#16611,#16612,#16613),(#16614,
#16615,#16616,#16617,#16618,#16619,#16620,#16621,#16622,#16623,#16624,#16625,
#16626,#16627,#16628,#16629,#16630,#16631,#16632,#16633,#16634,#16635,#16636,
#16637,#16638,#16639,#16640,#16641,#16642,#16643,#16644,#16645,#16646,#16647,
#16648),(#16649,#16650,#16651,#16652,#16653,#16654,#16655,#16656,#16657,
#16658,#16659,#16660,#16661,#16662,#16663,#16664,#16665,#16666,#16667,#16668,
#16669,#16670,#16671,#16672,#16673,#16674,#16675,#16676,#16677,#16678,#16679,
#16680,#16681,#16682,#16683)),.UNSPECIFIED.,.F.,.F.,.F.,(4,1,1,1,4),(4,
1,1,1,1,1,1,1,1,1,1,1,1,1,1,1,1,1,1,1,1,1,1,1,1,1,1,1,1,1,1,1,4),(0.4428548570514,
0.5,0.75,1.,1.057145142949),(-0.02,0.0125,0.045,0.0775,0.11,0.1425,0.175,
0.2075,0.24,0.2725,0.305,0.3375,0.37,0.4025,0.435,0.4675,0.5,0.5325,0.565,
0.5975,0.63,0.6625,0.695,0.7275,0.76,0.7925,0.825,0.8575,0.89,0.9225,0.955,
0.9875,1.02),.UNSPECIFIED.);
#17=ITEM_DEFINED_TRANSFORMATION($,$,#6242,#6553);
#18=ITEM_DEFINED_TRANSFORMATION($,$,#6301,#6554);
#19=ITEM_DEFINED_TRANSFORMATION($,$,#6523,#6555);
#20=ITEM_DEFINED_TRANSFORMATION($,$,#6523,#6556);
#21=ITEM_DEFINED_TRANSFORMATION($,$,#6610,#6697);
#22=ITEM_DEFINED_TRANSFORMATION($,$,#6652,#6698);
#23=ITEM_DEFINED_TRANSFORMATION($,$,#6679,#6699);
#24=ITEM_DEFINED_TRANSFORMATION($,$,#6558,#6700);
#25=ITEM_DEFINED_TRANSFORMATION($,$,#6609,#6701);
#26=ITEM_DEFINED_TRANSFORMATION($,$,#6836,#6923);
#27=ITEM_DEFINED_TRANSFORMATION($,$,#6881,#6924);
#28=ITEM_DEFINED_TRANSFORMATION($,$,#6901,#6925);
#29=ITEM_DEFINED_TRANSFORMATION($,$,#6703,#6926);
#30=ITEM_DEFINED_TRANSFORMATION($,$,#6781,#6927);
#31=ITEM_DEFINED_TRANSFORMATION($,$,#6815,#6928);
#32=ITEM_DEFINED_TRANSFORMATION($,$,#6818,#6929);
#33=ITEM_DEFINED_TRANSFORMATION($,$,#6835,#6930);
#34=ITEM_DEFINED_TRANSFORMATION($,$,#6210,#6973);
#35=ITEM_DEFINED_TRANSFORMATION($,$,#6241,#6974);
#36=ITEM_DEFINED_TRANSFORMATION($,$,#6557,#6975);
#37=ITEM_DEFINED_TRANSFORMATION($,$,#6702,#6976);
#38=ITEM_DEFINED_TRANSFORMATION($,$,#6931,#6977);
#39=(
REPRESENTATION_RELATIONSHIP($,$,#17187,#17186)
REPRESENTATION_RELATIONSHIP_WITH_TRANSFORMATION(#17)
SHAPE_REPRESENTATION_RELATIONSHIP()
);
#40=(
REPRESENTATION_RELATIONSHIP($,$,#17188,#17186)
REPRESENTATION_RELATIONSHIP_WITH_TRANSFORMATION(#18)
SHAPE_REPRESENTATION_RELATIONSHIP()
);
#41=(
REPRESENTATION_RELATIONSHIP($,$,#17189,#17186)
REPRESENTATION_RELATIONSHIP_WITH_TRANSFORMATION(#19)
SHAPE_REPRESENTATION_RELATIONSHIP()
);
#42=(
REPRESENTATION_RELATIONSHIP($,$,#17189,#17186)
REPRESENTATION_RELATIONSHIP_WITH_TRANSFORMATION(#20)
SHAPE_REPRESENTATION_RELATIONSHIP()
);
#43=(
REPRESENTATION_RELATIONSHIP($,$,#17193,#17192)
REPRESENTATION_RELATIONSHIP_WITH_TRANSFORMATION(#21)
SHAPE_REPRESENTATION_RELATIONSHIP()
);
#44=(
REPRESENTATION_RELATIONSHIP($,$,#17194,#17192)
REPRESENTATION_RELATIONSHIP_WITH_TRANSFORMATION(#22)
SHAPE_REPRESENTATION_RELATIONSHIP()
);
#45=(
REPRESENTATION_RELATIONSHIP($,$,#17195,#17192)
REPRESENTATION_RELATIONSHIP_WITH_TRANSFORMATION(#23)
SHAPE_REPRESENTATION_RELATIONSHIP()
);
#46=(
REPRESENTATION_RELATIONSHIP($,$,#17191,#17190)
REPRESENTATION_RELATIONSHIP_WITH_TRANSFORMATION(#24)
SHAPE_REPRESENTATION_RELATIONSHIP()
);
#47=(
REPRESENTATION_RELATIONSHIP($,$,#17192,#17190)
REPRESENTATION_RELATIONSHIP_WITH_TRANSFORMATION(#25)
SHAPE_REPRESENTATION_RELATIONSHIP()
);
#48=(
REPRESENTATION_RELATIONSHIP($,$,#17202,#17201)
REPRESENTATION_RELATIONSHIP_WITH_TRANSFORMATION(#26)
SHAPE_REPRESENTATION_RELATIONSHIP()
);
#49=(
REPRESENTATION_RELATIONSHIP($,$,#17203,#17201)
REPRESENTATION_RELATIONSHIP_WITH_TRANSFORMATION(#27)
SHAPE_REPRESENTATION_RELATIONSHIP()
);
#50=(
REPRESENTATION_RELATIONSHIP($,$,#17204,#17201)
REPRESENTATION_RELATIONSHIP_WITH_TRANSFORMATION(#28)
SHAPE_REPRESENTATION_RELATIONSHIP()
);
#51=(
REPRESENTATION_RELATIONSHIP($,$,#17197,#17196)
REPRESENTATION_RELATIONSHIP_WITH_TRANSFORMATION(#29)
SHAPE_REPRESENTATION_RELATIONSHIP()
);
#52=(
REPRESENTATION_RELATIONSHIP($,$,#17198,#17196)
REPRESENTATION_RELATIONSHIP_WITH_TRANSFORMATION(#30)
SHAPE_REPRESENTATION_RELATIONSHIP()
);
#53=(
REPRESENTATION_RELATIONSHIP($,$,#17199,#17196)
REPRESENTATION_RELATIONSHIP_WITH_TRANSFORMATION(#31)
SHAPE_REPRESENTATION_RELATIONSHIP()
);
#54=(
REPRESENTATION_RELATIONSHIP($,$,#17200,#17196)
REPRESENTATION_RELATIONSHIP_WITH_TRANSFORMATION(#32)
SHAPE_REPRESENTATION_RELATIONSHIP()
);
#55=(
REPRESENTATION_RELATIONSHIP($,$,#17201,#17196)
REPRESENTATION_RELATIONSHIP_WITH_TRANSFORMATION(#33)
SHAPE_REPRESENTATION_RELATIONSHIP()
);
#56=(
REPRESENTATION_RELATIONSHIP($,$,#17185,#17184)
REPRESENTATION_RELATIONSHIP_WITH_TRANSFORMATION(#34)
SHAPE_REPRESENTATION_RELATIONSHIP()
);
#57=(
REPRESENTATION_RELATIONSHIP($,$,#17186,#17184)
REPRESENTATION_RELATIONSHIP_WITH_TRANSFORMATION(#35)
SHAPE_REPRESENTATION_RELATIONSHIP()
);
#58=(
REPRESENTATION_RELATIONSHIP($,$,#17190,#17184)
REPRESENTATION_RELATIONSHIP_WITH_TRANSFORMATION(#36)
SHAPE_REPRESENTATION_RELATIONSHIP()
);
#59=(
REPRESENTATION_RELATIONSHIP($,$,#17196,#17184)
REPRESENTATION_RELATIONSHIP_WITH_TRANSFORMATION(#37)
SHAPE_REPRESENTATION_RELATIONSHIP()
);
#60=(
REPRESENTATION_RELATIONSHIP($,$,#17205,#17184)
REPRESENTATION_RELATIONSHIP_WITH_TRANSFORMATION(#38)
SHAPE_REPRESENTATION_RELATIONSHIP()
);
#61=CONTEXT_DEPENDENT_SHAPE_REPRESENTATION(#39,#17146);
#62=CONTEXT_DEPENDENT_SHAPE_REPRESENTATION(#40,#17147);
#63=CONTEXT_DEPENDENT_SHAPE_REPRESENTATION(#41,#17148);
#64=CONTEXT_DEPENDENT_SHAPE_REPRESENTATION(#42,#17149);
#65=CONTEXT_DEPENDENT_SHAPE_REPRESENTATION(#43,#17156);
#66=CONTEXT_DEPENDENT_SHAPE_REPRESENTATION(#44,#17157);
#67=CONTEXT_DEPENDENT_SHAPE_REPRESENTATION(#45,#17158);
#68=CONTEXT_DEPENDENT_SHAPE_REPRESENTATION(#46,#17159);
#69=CONTEXT_DEPENDENT_SHAPE_REPRESENTATION(#47,#17160);
#70=CONTEXT_DEPENDENT_SHAPE_REPRESENTATION(#48,#17170);
#71=CONTEXT_DEPENDENT_SHAPE_REPRESENTATION(#49,#17171);
#72=CONTEXT_DEPENDENT_SHAPE_REPRESENTATION(#50,#17172);
#73=CONTEXT_DEPENDENT_SHAPE_REPRESENTATION(#51,#17173);
#74=CONTEXT_DEPENDENT_SHAPE_REPRESENTATION(#52,#17174);
#75=CONTEXT_DEPENDENT_SHAPE_REPRESENTATION(#53,#17175);
#76=CONTEXT_DEPENDENT_SHAPE_REPRESENTATION(#54,#17176);
#77=CONTEXT_DEPENDENT_SHAPE_REPRESENTATION(#55,#17177);
#78=CONTEXT_DEPENDENT_SHAPE_REPRESENTATION(#56,#17179);
#79=CONTEXT_DEPENDENT_SHAPE_REPRESENTATION(#57,#17180);
#80=CONTEXT_DEPENDENT_SHAPE_REPRESENTATION(#58,#17181);
#81=CONTEXT_DEPENDENT_SHAPE_REPRESENTATION(#59,#17182);
#82=CONTEXT_DEPENDENT_SHAPE_REPRESENTATION(#60,#17183);
#83=NEXT_ASSEMBLY_USAGE_OCCURRENCE('BASEPLATE:1','BASEPLATE:1',
'BASEPLATE:1',#17209,#17210,'BASEPLATE:1');
#84=NEXT_ASSEMBLY_USAGE_OCCURRENCE('COLUMN:1','COLUMN:1','COLUMN:1',#17209,
#17211,'COLUMN:1');
#85=NEXT_ASSEMBLY_USAGE_OCCURRENCE('IN-OUTLET:1','IN-OUTLET:1',
'IN-OUTLET:1',#17209,#17212,'IN-OUTLET:1');
#86=NEXT_ASSEMBLY_USAGE_OCCURRENCE('IN-OUTLET:2','IN-OUTLET:2',
'IN-OUTLET:2',#17209,#17212,'IN-OUTLET:2');
#87=NEXT_ASSEMBLY_USAGE_OCCURRENCE('7-2:1','7-2:1','7-2:1',#17215,#17216,
'7-2:1');
#88=NEXT_ASSEMBLY_USAGE_OCCURRENCE('7-1:1','7-1:1','7-1:1',#17215,#17217,
'7-1:1');
#89=NEXT_ASSEMBLY_USAGE_OCCURRENCE('7-3:1','7-3:1','7-3:1',#17215,#17218,
'7-3:1');
#90=NEXT_ASSEMBLY_USAGE_OCCURRENCE('FLYWHEEL:1','FLYWHEEL:1',
'FLYWHEEL:1',#17213,#17214,'FLYWHEEL:1');
#91=NEXT_ASSEMBLY_USAGE_OCCURRENCE('CRANKSHAFT_ASM:1',
'CRANKSHAFT_ASM:1','CRANKSHAFT_ASM:1',#17213,#17215,'CRANKSHAFT_ASM:1');
#92=NEXT_ASSEMBLY_USAGE_OCCURRENCE('6-1:1','6-1:1','6-1:1',#17224,#17225,
'6-1:1');
#93=NEXT_ASSEMBLY_USAGE_OCCURRENCE('6-2:1','6-2:1','6-2:1',#17224,#17226,
'6-2:1');
#94=NEXT_ASSEMBLY_USAGE_OCCURRENCE('6-3:1','6-3:1','6-3:1',#17224,#17227,
'6-3:1');
#95=NEXT_ASSEMBLY_USAGE_OCCURRENCE('CYLINDER:1','CYLINDER:1',
'CYLINDER:1',#17219,#17220,'CYLINDER:1');
#96=NEXT_ASSEMBLY_USAGE_OCCURRENCE('CYLINDERCOVER:1','CYLINDERCOVER:1',
'CYLINDERCOVER:1',#17219,#17221,'CYLINDERCOVER:1');
#97=NEXT_ASSEMBLY_USAGE_OCCURRENCE('PRESSURESPRING:1',
'PRESSURESPRING:1','PRESSURESPRING:1',#17219,#17222,'PRESSURESPRING:1');
#98=NEXT_ASSEMBLY_USAGE_OCCURRENCE('NUT:1','NUT:1','NUT:1',#17219,#17223,
'NUT:1');
#99=NEXT_ASSEMBLY_USAGE_OCCURRENCE('PISTON_ASM:1','PISTON_ASM:1',
'PISTON_ASM:1',#17219,#17224,'PISTON_ASM:1');
#100=NEXT_ASSEMBLY_USAGE_OCCURRENCE('BASE:1','BASE:1','BASE:1',#17207,#17208,
'BASE:1');
#101=NEXT_ASSEMBLY_USAGE_OCCURRENCE('1_ASM:1','1_ASM:1','1_ASM:1',#17207,
#17209,'1_ASM:1');
#102=NEXT_ASSEMBLY_USAGE_OCCURRENCE('3_ASM:1','3_ASM:1','3_ASM:1',#17207,
#17213,'3_ASM:1');
#103=NEXT_ASSEMBLY_USAGE_OCCURRENCE('2_ASM:1','2_ASM:1','2_ASM:1',#17207,
#17219,'2_ASM:1');
#104=NEXT_ASSEMBLY_USAGE_OCCURRENCE('NAMEPLATE:1','NAMEPLATE:1',
'NAMEPLATE:1',#17207,#17228,'NAMEPLATE:1');
#105=ELLIPSE('',#6445,1.4142135623731,1.);
#106=ELLIPSE('',#6457,1.41421356237309,1.);
#107=ELLIPSE('',#6627,1.26223360526973,1.25);
#108=ELLIPSE('',#6640,1.26223360526973,1.25);
#109=(
BOUNDED_SURFACE()
B_SPLINE_SURFACE(3,3,((#9243,#9244,#9245,#9246,#9247,#9248,#9249,#9250,
#9251,#9252,#9253,#9254,#9255),(#9256,#9257,#9258,#9259,#9260,#9261,#9262,
#9263,#9264,#9265,#9266,#9267,#9268),(#9269,#9270,#9271,#9272,#9273,#9274,
#9275,#9276,#9277,#9278,#9279,#9280,#9281),(#9282,#9283,#9284,#9285,#9286,
#9287,#9288,#9289,#9290,#9291,#9292,#9293,#9294)),.UNSPECIFIED.,.F.,.F.,
 .F.)
B_SPLINE_SURFACE_WITH_KNOTS((4,4),(4,1,1,1,1,1,1,1,1,1,4),(0.,1.),(-0.01854087386661,
0.,0.124538046056,0.2354380828125,0.3411963661322,0.4510248812945,0.5701285898783,
0.7002368466242,0.8429884965965,1.,1.018551127109),.UNSPECIFIED.)
GEOMETRIC_REPRESENTATION_ITEM()
RATIONAL_B_SPLINE_SURFACE(((1.236576476327,1.236576476327,1.236576476327,
1.236576476327,1.236576476327,1.236576476327,1.236576476327,1.236576476327,
1.236576476327,1.236576476327,1.236576476327,1.236576476327,1.236576476327),
(0.9211411745578,0.9211411745578,0.9211411745578,0.9211411745578,0.9211411745578,
0.9211411745578,0.9211411745578,0.9211411745578,0.9211411745578,0.9211411745578,
0.9211411745578,0.9211411745578,0.9211411745578),(0.9211411745578,0.9211411745578,
0.9211411745578,0.9211411745578,0.9211411745578,0.9211411745578,0.9211411745578,
0.9211411745578,0.9211411745578,0.9211411745578,0.9211411745578,0.9211411745578,
0.9211411745578),(1.236576476327,1.236576476327,1.236576476327,1.236576476327,
1.236576476327,1.236576476327,1.236576476327,1.236576476327,1.236576476327,
1.236576476327,1.236576476327,1.236576476327,1.236576476327)))
REPRESENTATION_ITEM('')
SURFACE()
);
#110=(
BOUNDED_SURFACE()
B_SPLINE_SURFACE(3,3,((#9423,#9424,#9425,#9426,#9427,#9428,#9429,#9430,
#9431,#9432,#9433,#9434,#9435),(#9436,#9437,#9438,#9439,#9440,#9441,#9442,
#9443,#9444,#9445,#9446,#9447,#9448),(#9449,#9450,#9451,#9452,#9453,#9454,
#9455,#9456,#9457,#9458,#9459,#9460,#9461),(#9462,#9463,#9464,#9465,#9466,
#9467,#9468,#9469,#9470,#9471,#9472,#9473,#9474)),.UNSPECIFIED.,.F.,.F.,
 .F.)
B_SPLINE_SURFACE_WITH_KNOTS((4,4),(4,1,1,1,1,1,1,1,1,1,4),(0.,1.),(-0.01854087386661,
0.,0.124538046056,0.2354380828125,0.3411963661322,0.4510248812945,0.5701285898783,
0.7002368466242,0.8429884965965,1.,1.018551127109),.UNSPECIFIED.)
GEOMETRIC_REPRESENTATION_ITEM()
RATIONAL_B_SPLINE_SURFACE(((1.236576476327,1.236576476327,1.236576476327,
1.236576476327,1.236576476327,1.236576476327,1.236576476327,1.236576476327,
1.236576476327,1.236576476327,1.236576476327,1.236576476327,1.236576476327),
(0.9211411745578,0.9211411745578,0.9211411745578,0.9211411745578,0.9211411745578,
0.9211411745578,0.9211411745578,0.9211411745578,0.9211411745578,0.9211411745578,
0.9211411745578,0.9211411745578,0.9211411745578),(0.9211411745578,0.9211411745578,
0.9211411745578,0.9211411745578,0.9211411745578,0.9211411745578,0.9211411745578,
0.9211411745578,0.9211411745578,0.9211411745578,0.9211411745578,0.9211411745578,
0.9211411745578),(1.236576476327,1.236576476327,1.236576476327,1.236576476327,
1.236576476327,1.236576476327,1.236576476327,1.236576476327,1.236576476327,
1.236576476327,1.236576476327,1.236576476327,1.236576476327)))
REPRESENTATION_ITEM('')
SURFACE()
);
#111=(
BOUNDED_SURFACE()
B_SPLINE_SURFACE(3,3,((#9791,#9792,#9793,#9794,#9795,#9796,#9797,#9798,
#9799,#9800,#9801,#9802,#9803,#9804,#9805,#9806,#9807),(#9808,#9809,#9810,
#9811,#9812,#9813,#9814,#9815,#9816,#9817,#9818,#9819,#9820,#9821,#9822,
#9823,#9824),(#9825,#9826,#9827,#9828,#9829,#9830,#9831,#9832,#9833,#9834,
#9835,#9836,#9837,#9838,#9839,#9840,#9841),(#9842,#9843,#9844,#9845,#9846,
#9847,#9848,#9849,#9850,#9851,#9852,#9853,#9854,#9855,#9856,#9857,#9858)),
 .UNSPECIFIED.,.F.,.F.,.F.)
B_SPLINE_SURFACE_WITH_KNOTS((4,4),(4,1,1,1,1,1,1,1,1,1,1,1,1,1,4),(0.,1.),
(-0.009903506240665,0.,0.09441816002876,0.1881578788494,0.280939071815,
0.3715247502583,0.4641517260557,0.5619785611963,0.6570408645664,0.7414898315922,
0.8160167895793,0.8826179898193,0.9432826185749,1.,1.009908876933),
 .UNSPECIFIED.)
GEOMETRIC_REPRESENTATION_ITEM()
RATIONAL_B_SPLINE_SURFACE(((1.236576619558,1.236576619558,1.236576619558,
1.236576619558,1.236576619558,1.236576619558,1.236576619558,1.236576619558,
1.236576619558,1.236576619558,1.236576619558,1.236576619558,1.236576619558,
1.236576619558,1.236576619558,1.236576619558,1.236576619558),(0.9211411268139,
0.9211411268139,0.9211411268139,0.9211411268139,0.9211411268139,0.9211411268139,
0.9211411268139,0.9211411268139,0.9211411268139,0.9211411268139,0.9211411268139,
0.9211411268139,0.9211411268139,0.9211411268139,0.9211411268139,0.9211411268139,
0.9211411268139),(0.9211411268139,0.9211411268139,0.9211411268139,0.9211411268139,
0.9211411268139,0.9211411268139,0.9211411268139,0.9211411268139,0.9211411268139,
0.9211411268139,0.9211411268139,0.9211411268139,0.9211411268139,0.9211411268139,
0.9211411268139,0.9211411268139,0.9211411268139),(1.236576619558,1.236576619558,
1.236576619558,1.236576619558,1.236576619558,1.236576619558,1.236576619558,
1.236576619558,1.236576619558,1.236576619558,1.236576619558,1.236576619558,
1.236576619558,1.236576619558,1.236576619558,1.236576619558,1.236576619558)))
REPRESENTATION_ITEM('')
SURFACE()
);
#112=(
BOUNDED_SURFACE()
B_SPLINE_SURFACE(3,3,((#10155,#10156,#10157,#10158,#10159,#10160,#10161,
#10162,#10163,#10164,#10165),(#10166,#10167,#10168,#10169,#10170,#10171,
#10172,#10173,#10174,#10175,#10176),(#10177,#10178,#10179,#10180,#10181,
#10182,#10183,#10184,#10185,#10186,#10187),(#10188,#10189,#10190,#10191,
#10192,#10193,#10194,#10195,#10196,#10197,#10198)),.UNSPECIFIED.,.F.,.F.,
 .F.)
B_SPLINE_SURFACE_WITH_KNOTS((4,4),(4,1,1,1,1,1,1,1,4),(0.,1.),(-0.0117961357116,
0.,0.1633770608974,0.3160773256608,0.4701362865974,0.6315432333968,0.8054144885927,
1.,1.011975292336),.UNSPECIFIED.)
GEOMETRIC_REPRESENTATION_ITEM()
RATIONAL_B_SPLINE_SURFACE(((1.236576493506,1.236576493506,1.236576493506,
1.236576493506,1.236576493506,1.236576493506,1.236576493506,1.236576493506,
1.236576493506,1.236576493506,1.236576493506),(0.9211411688312,0.9211411688312,
0.9211411688312,0.9211411688312,0.9211411688312,0.9211411688312,0.9211411688312,
0.9211411688312,0.9211411688312,0.9211411688312,0.9211411688312),(0.9211411688312,
0.9211411688312,0.9211411688312,0.9211411688312,0.9211411688312,0.9211411688312,
0.9211411688312,0.9211411688312,0.9211411688312,0.9211411688312,0.9211411688312),
(1.236576493506,1.236576493506,1.236576493506,1.236576493506,1.236576493506,
1.236576493506,1.236576493506,1.236576493506,1.236576493506,1.236576493506,
1.236576493506)))
REPRESENTATION_ITEM('')
SURFACE()
);
#113=(
BOUNDED_SURFACE()
B_SPLINE_SURFACE(3,3,((#10200,#10201,#10202,#10203,#10204,#10205,#10206,
#10207,#10208,#10209,#10210,#10211,#10212),(#10213,#10214,#10215,#10216,
#10217,#10218,#10219,#10220,#10221,#10222,#10223,#10224,#10225),(#10226,
#10227,#10228,#10229,#10230,#10231,#10232,#10233,#10234,#10235,#10236,#10237,
#10238),(#10239,#10240,#10241,#10242,#10243,#10244,#10245,#10246,#10247,
#10248,#10249,#10250,#10251)),.UNSPECIFIED.,.F.,.F.,.F.)
B_SPLINE_SURFACE_WITH_KNOTS((4,4),(4,1,1,1,1,1,1,1,1,1,4),(0.,1.),(-0.02387271189713,
0.,0.1233219598256,0.2447228034141,0.3668475159477,0.4855515195745,0.6022629448181,
0.7239422574426,0.8555602069799,1.,1.011825585123),.UNSPECIFIED.)
GEOMETRIC_REPRESENTATION_ITEM()
RATIONAL_B_SPLINE_SURFACE(((1.236576471212,1.236576471212,1.236576471212,
1.236576471212,1.236576471212,1.236576471212,1.236576471212,1.236576471212,
1.236576471212,1.236576471212,1.236576471212,1.236576471212,1.236576471212),
(0.9211411762628,0.9211411762628,0.9211411762628,0.9211411762628,0.9211411762628,
0.9211411762628,0.9211411762628,0.9211411762628,0.9211411762628,0.9211411762628,
0.9211411762628,0.9211411762628,0.9211411762628),(0.9211411762628,0.9211411762628,
0.9211411762628,0.9211411762628,0.9211411762628,0.9211411762628,0.9211411762628,
0.9211411762628,0.9211411762628,0.9211411762628,0.9211411762628,0.9211411762628,
0.9211411762628),(1.236576471212,1.236576471212,1.236576471212,1.236576471212,
1.236576471212,1.236576471212,1.236576471212,1.236576471212,1.236576471212,
1.236576471212,1.236576471212,1.236576471212,1.236576471212)))
REPRESENTATION_ITEM('')
SURFACE()
);
#114=SPHERICAL_SURFACE('',#6330,1.);
#115=SPHERICAL_SURFACE('',#6351,1.);
#116=SPHERICAL_SURFACE('',#6354,1.);
#117=SPHERICAL_SURFACE('',#6359,1.);
#118=SPHERICAL_SURFACE('',#6367,1.);
#119=SPHERICAL_SURFACE('',#6371,1.);
#120=SPHERICAL_SURFACE('',#6382,1.);
#121=SPHERICAL_SURFACE('',#6383,1.);
#122=SPHERICAL_SURFACE('',#6480,1.);
#123=SPHERICAL_SURFACE('',#6487,1.);
#124=SPHERICAL_SURFACE('',#6499,1.);
#125=SPHERICAL_SURFACE('',#6505,1.);
#126=TOROIDAL_SURFACE('',#6307,4.,0.5);
#127=TOROIDAL_SURFACE('',#6316,4.,0.5);
#128=TOROIDAL_SURFACE('',#6343,6.217106130074,3.);
#129=TOROIDAL_SURFACE('',#6401,6.,3.);
#130=TOROIDAL_SURFACE('',#6403,12.13789139507,5.);
#131=TOROIDAL_SURFACE('',#6435,2.,1.);
#132=TOROIDAL_SURFACE('',#6459,2.,1.);
#133=TOROIDAL_SURFACE('',#6492,2.,1.);
#134=TOROIDAL_SURFACE('',#6509,2.,1.);
#135=TOROIDAL_SURFACE('',#6625,6.5,0.5);
#136=TOROIDAL_SURFACE('',#6631,5.7,0.3);
#137=TOROIDAL_SURFACE('',#6636,3.2,0.3);
#138=TOROIDAL_SURFACE('',#6725,15.5,0.5);
#139=TOROIDAL_SURFACE('',#6736,11.,0.5);
#140=TOROIDAL_SURFACE('',#6744,10.9999999985,0.5);
#141=TOROIDAL_SURFACE('',#6748,10.,0.5);
#142=TOROIDAL_SURFACE('',#6796,6.,1.);
#143=TOROIDAL_SURFACE('',#6810,15.5,0.5);
#144=TOROIDAL_SURFACE('',#6864,4.5,1.);
#145=TOROIDAL_SURFACE('',#6870,4.5,1.);
#146=B_SPLINE_CURVE_WITH_KNOTS('',3,(#9111,#9112,#9113,#9114,#9115,#9116,
#9117,#9118,#9119,#9120,#9121),.UNSPECIFIED.,.F.,.F.,(4,1,1,1,1,1,1,1,4),
(5.02030750257932E-6,0.125,0.25,0.375,0.5,0.625,0.75,0.875,1.),
 .UNSPECIFIED.);
#147=B_SPLINE_CURVE_WITH_KNOTS('',3,(#9146,#9147,#9148,#9149,#9150,#9151,
#9152,#9153,#9154,#9155,#9156,#9157,#9158,#9159,#9160,#9161,#9162,#9163),
 .UNSPECIFIED.,.F.,.F.,(4,2,2,2,2,2,2,2,4),(0.38439055210377,0.432504952213954,
0.480619352324138,0.528602590239896,0.576585828155655,0.624569066071413,
0.672552303987171,0.720666704097356,0.76878110420754),.UNSPECIFIED.);
#148=B_SPLINE_CURVE_WITH_KNOTS('',3,(#9164,#9165,#9166,#9167,#9168,#9169,
#9170,#9171,#9172,#9173,#9174,#9175,#9176,#9177,#9178,#9179,#9180,#9181),
 .UNSPECIFIED.,.F.,.F.,(4,2,2,2,2,2,2,2,4),(0.76878110420754,0.816895504317724,
0.865009904427908,0.912993142343666,0.960976380259425,1.00895961817518,
1.05694285609094,1.10505725620113,1.15317165631131),.UNSPECIFIED.);
#149=B_SPLINE_CURVE_WITH_KNOTS('',3,(#9206,#9207,#9208,#9209,#9210,#9211,
#9212,#9213,#9214,#9215,#9216),.UNSPECIFIED.,.F.,.F.,(4,1,1,1,1,1,1,1,4),
(5.02030750249862E-6,0.125,0.25,0.375,0.5,0.625,0.75,0.875,1.),
 .UNSPECIFIED.);
#150=B_SPLINE_CURVE_WITH_KNOTS('',3,(#9296,#9297,#9298,#9299,#9300,#9301,
#9302,#9303,#9304,#9305,#9306,#9307,#9308,#9309,#9310,#9311,#9312,#9313,
#9314,#9315,#9316,#9317,#9318,#9319,#9320,#9321,#9322,#9323,#9324,#9325,
#9326,#9327,#9328,#9329,#9330,#9331,#9332,#9333,#9334,#9335,#9336,#9337,
#9338,#9339,#9340,#9341,#9342,#9343,#9344),.UNSPECIFIED.,.F.,.F.,(4,3,3,
3,3,3,3,3,3,3,3,3,3,3,3,3,4),(4.37386987750375E-6,0.0927050507258515,0.125,
0.21480736126803,0.25,0.35993980774069,0.375,0.491161389173609,0.5,0.611281050311693,
0.625,0.72687460423662,0.75,0.841555339636589,0.875,0.952466785368161,1.),
 .UNSPECIFIED.);
#151=B_SPLINE_CURVE_WITH_KNOTS('',3,(#9368,#9369,#9370,#9371,#9372,#9373,
#9374,#9375,#9376,#9377,#9378,#9379,#9380,#9381,#9382,#9383,#9384,#9385,
#9386,#9387,#9388,#9389,#9390,#9391,#9392,#9393,#9394,#9395,#9396,#9397,
#9398,#9399,#9400,#9401,#9402,#9403,#9404,#9405,#9406,#9407,#9408,#9409,
#9410,#9411,#9412,#9413,#9414,#9415,#9416,#9417,#9418,#9419,#9420,#9421,
#9422),.UNSPECIFIED.,.F.,.F.,(4,3,3,3,3,3,3,3,3,3,3,3,3,3,3,3,3,3,4),(4.37386990229217E-6,
0.078116780989183,0.125,0.178786314155506,0.234096638055846,0.25,0.307075966738911,
0.364185364927029,0.375,0.440633200921451,0.5,0.585859467132409,0.625,0.699968906702808,
0.75,0.824334220487127,0.875,0.940179003774522,1.),.UNSPECIFIED.);
#152=B_SPLINE_CURVE_WITH_KNOTS('',3,(#9566,#9567,#9568,#9569,#9570,#9571,
#9572,#9573,#9574,#9575),.UNSPECIFIED.,.F.,.F.,(4,2,2,2,4),(5.976817519871,
6.14313994502015,6.3094623701693,6.59082757274907,6.87100413233151),
 .UNSPECIFIED.);
#153=B_SPLINE_CURVE_WITH_KNOTS('',3,(#9579,#9580,#9581,#9582,#9583,#9584,
#9585,#9586,#9587,#9588,#9589,#9590,#9591,#9592,#9593,#9594,#9595,#9596,
#9597,#9598,#9599,#9600,#9601,#9602,#9603,#9604,#9605,#9606,#9607,#9608,
#9609,#9610,#9611,#9612,#9613,#9614,#9615,#9616,#9617,#9618,#9619,#9620,
#9621),.UNSPECIFIED.,.F.,.F.,(4,3,3,3,3,3,3,3,3,3,3,3,3,3,4),(4.15972417351908E-9,
0.0998336668422238,0.1666666666667,0.243344677320033,0.328047736632198,
0.3333333333333,0.448940244692513,0.5,0.600185553237847,0.6666666666667,
0.75,0.825496133016552,0.8333333333333,0.92981319294891,0.999999999596363),
 .UNSPECIFIED.);
#154=B_SPLINE_CURVE_WITH_KNOTS('',3,(#9623,#9624,#9625,#9626,#9627,#9628,
#9629,#9630,#9631,#9632,#9633,#9634,#9635,#9636,#9637,#9638,#9639,#9640,
#9641,#9642,#9643,#9644,#9645,#9646,#9647,#9648,#9649,#9650,#9651,#9652,
#9653,#9654,#9655,#9656,#9657,#9658,#9659,#9660,#9661,#9662,#9663,#9664,
#9665,#9666,#9667,#9668),.UNSPECIFIED.,.F.,.F.,(4,3,3,3,3,3,3,3,3,3,3,3,
3,3,3,4),(0.,0.125,0.210638947521259,0.25,0.337872505342455,0.375,0.480596631880562,
0.5,0.597224358508775,0.625,0.710418048307479,0.75,0.823358228203642,0.875,
0.94278763723167,0.999999999303434),.UNSPECIFIED.);
#155=B_SPLINE_CURVE_WITH_KNOTS('',3,(#9672,#9673,#9674,#9675,#9676,#9677,
#9678,#9679,#9680,#9681,#9682,#9683,#9684,#9685,#9686,#9687,#9688,#9689,
#9690),.UNSPECIFIED.,.F.,.F.,(4,2,2,2,3,2,2,2,4),(-0.895375255457832,-0.72905283030868,
-0.562730405159529,-0.281365202579764,0.,0.281365202579765,0.562730405159529,
0.729052830308681,0.895375255457832),.UNSPECIFIED.);
#156=B_SPLINE_CURVE_WITH_KNOTS('',3,(#9694,#9695,#9696,#9697,#9698,#9699,
#9700,#9701,#9702,#9703,#9704,#9705,#9706,#9707,#9708,#9709,#9710,#9711,
#9712,#9713,#9714,#9715,#9716,#9717,#9718,#9719,#9720,#9721,#9722,#9723,
#9724,#9725,#9726,#9727,#9728,#9729,#9730,#9731,#9732,#9733,#9734,#9735,
#9736,#9737,#9738,#9739,#9740,#9741,#9742,#9743,#9744,#9745,#9746,#9747,
#9748,#9749,#9750,#9751,#9752,#9753,#9754,#9755,#9756,#9757,#9758,#9759,
#9760,#9761,#9762,#9763,#9764,#9765,#9766,#9767,#9768,#9769,#9770,#9771,
#9772,#9773,#9774,#9775),.UNSPECIFIED.,.F.,.F.,(4,3,3,3,3,3,3,3,3,3,3,3,
3,3,3,3,3,3,3,3,3,3,3,3,3,3,3,4),(0.,0.0559513285251171,0.08333333333333,
0.1666666666667,0.216931260660868,0.25,0.294848169718225,0.3333333333333,
0.375,0.413940896871108,0.4166666666667,0.451751192947467,0.486849107740909,
0.5,0.53799564679006,0.577957191404146,0.5833333333333,0.622184542089551,
0.663983458717584,0.6666666666667,0.712268138213338,0.75,0.801593987292321,
0.8333333333333,0.893036722145433,0.9166666666667,0.97337992594817,0.999999974018396),
 .UNSPECIFIED.);
#157=B_SPLINE_CURVE_WITH_KNOTS('',3,(#9778,#9779,#9780,#9781,#9782,#9783,
#9784,#9785,#9786,#9787,#9788,#9789,#9790),.UNSPECIFIED.,.F.,.F.,(4,3,2,
2,2,4),(6.87100413233151,6.87219277532883,7.1535579779086,7.43492318048836,
7.60124560563752,7.76756803078667),.UNSPECIFIED.);
#158=B_SPLINE_CURVE_WITH_KNOTS('',3,(#9861,#9862,#9863,#9864,#9865,#9866,
#9867,#9868,#9869,#9870,#9871,#9872,#9873,#9874,#9875),.UNSPECIFIED.,.F.,
 .F.,(4,1,1,1,1,1,1,1,1,1,1,1,4),(4.80530147585308E-8,0.08333333333333,
0.1666666666667,0.25,0.3333333333333,0.4166666666667,0.5,0.5833333333333,
0.6666666666667,0.75,0.8333333333333,0.9166666666667,0.999999273982094),
 .UNSPECIFIED.);
#159=B_SPLINE_CURVE_WITH_KNOTS('',3,(#9904,#9905,#9906,#9907),
 .UNSPECIFIED.,.F.,.F.,(4,4),(0.779469865639367,0.833309307571144),
 .UNSPECIFIED.);
#160=B_SPLINE_CURVE_WITH_KNOTS('',3,(#9909,#9910,#9911,#9912,#9913,#9914,
#9915,#9916,#9917,#9918,#9919,#9920,#9921,#9922,#9923,#9924,#9925,#9926,
#9927,#9928,#9929,#9930,#9931,#9932,#9933),.UNSPECIFIED.,.F.,.F.,(4,2,2,
2,2,3,2,2,2,2,2,4),(0.833309307571144,0.908998418331253,0.984687529091362,
1.05819154321553,1.09494355027761,1.13169555733969,1.16844756440177,1.20519957146385,
1.27870358558802,1.35439269634812,1.43008180710823,1.48392124906823),
 .UNSPECIFIED.);
#161=B_SPLINE_CURVE_WITH_KNOTS('',3,(#9937,#9938,#9939,#9940,#9941,#9942,
#9943,#9944,#9945,#9946,#9947,#9948,#9949,#9950,#9951,#9952,#9953,#9954),
 .UNSPECIFIED.,.F.,.F.,(4,2,2,2,2,2,2,2,4),(0.352225691728541,0.364327757248449,
0.430269264728352,0.498058521699098,0.565847778669844,0.63363703564059,
0.701426292611336,0.76736780009124,0.779469865639367),.UNSPECIFIED.);
#162=B_SPLINE_CURVE_WITH_KNOTS('',3,(#9979,#9980,#9981,#9982,#9983,#9984),
 .UNSPECIFIED.,.F.,.F.,(4,2,4),(0.,0.117562819132916,0.19402604569559),
 .UNSPECIFIED.);
#163=B_SPLINE_CURVE_WITH_KNOTS('',3,(#9995,#9996,#9997,#9998,#9999,#10000),
 .UNSPECIFIED.,.F.,.F.,(4,2,4),(0.505532240038497,0.581995466601172,0.699558285734087),
 .UNSPECIFIED.);
#164=B_SPLINE_CURVE_WITH_KNOTS('',3,(#10006,#10007,#10008,#10009,#10010,
#10011,#10012,#10013,#10014,#10015,#10016,#10017,#10018,#10019,#10020,#10021,
#10022,#10023,#10024,#10025,#10026,#10027,#10028),.UNSPECIFIED.,.F.,.F.,
(4,2,2,2,2,3,2,2,2,2,4),(0.833309307571144,0.908998418331253,0.984687529091362,
1.05819154321553,1.09494355027761,1.13169555733969,1.16844756440177,1.20519957146385,
1.27870358558802,1.35439269634812,1.43008180710823),.UNSPECIFIED.);
#165=B_SPLINE_CURVE_WITH_KNOTS('',3,(#10031,#10032,#10033,#10034),
 .UNSPECIFIED.,.F.,.F.,(4,4),(1.43008180710823,1.48392124904001),
 .UNSPECIFIED.);
#166=B_SPLINE_CURVE_WITH_KNOTS('',3,(#10036,#10037,#10038,#10039,#10040,
#10041,#10042,#10043,#10044,#10045,#10046,#10047,#10048,#10049,#10050,#10051,
#10052,#10053),.UNSPECIFIED.,.F.,.F.,(4,2,2,2,2,2,2,2,4),(1.48392124904001,
1.49602331458814,1.56196482206804,1.62975407903879,1.69754333600953,1.76533259298028,
1.83312184995102,1.89906335743093,1.91116542297906),.UNSPECIFIED.);
#167=B_SPLINE_CURVE_WITH_KNOTS('',3,(#10054,#10055,#10056,#10057),
 .UNSPECIFIED.,.F.,.F.,(4,4),(1.91116542297906,1.96500486491083),
 .UNSPECIFIED.);
#168=B_SPLINE_CURVE_WITH_KNOTS('',3,(#10074,#10075,#10076,#10077,#10078,
#10079,#10080,#10081,#10082,#10083,#10084),.UNSPECIFIED.,.F.,.F.,(4,1,1,
1,1,1,1,1,4),(0.,0.125,0.25,0.375,0.5,0.625,0.75,0.875,0.999999972808484),
 .UNSPECIFIED.);
#169=B_SPLINE_CURVE_WITH_KNOTS('',3,(#10086,#10087,#10088,#10089,#10090,
#10091,#10092,#10093,#10094),.UNSPECIFIED.,.F.,.F.,(4,1,1,1,1,1,4),(1.77479359457994E-7,
0.1666666666667,0.3333333333333,0.5,0.6666666666667,0.8333333333333,1.),
 .UNSPECIFIED.);
#170=B_SPLINE_CURVE_WITH_KNOTS('',3,(#10460,#10461,#10462,#10463,#10464,
#10465,#10466,#10467,#10468,#10469,#10470,#10471,#10472,#10473,#10474,#10475,
#10476,#10477),.UNSPECIFIED.,.F.,.F.,(4,2,2,2,2,2,2,2,4),(-0.567632662698663,
-0.520333247919949,-0.473033833141235,-0.425727804136839,-0.378421775132442,
-0.331115746128045,-0.283809717123649,-0.236510302344935,-0.189210887566221),
 .UNSPECIFIED.);
#171=B_SPLINE_CURVE_WITH_KNOTS('',3,(#10478,#10479,#10480,#10481,#10482,
#10483,#10484,#10485,#10486,#10487,#10488,#10489,#10490,#10491,#10492,#10493,
#10494,#10495,#10496),.UNSPECIFIED.,.F.,.F.,(4,2,2,2,3,2,2,2,4),(-0.189210887566221,
-0.141911472787507,-0.0946120580087934,-0.0473060290043967,0.,0.0473060290043967,
0.0946120580087935,0.141911472787507,0.189210887566221),.UNSPECIFIED.);
#172=B_SPLINE_CURVE_WITH_KNOTS('',3,(#10498,#10499,#10500,#10501,#10502,
#10503,#10504,#10505,#10506,#10507,#10508,#10509,#10510,#10511,#10512,#10513,
#10514,#10515,#10516,#10517,#10518,#10519,#10520,#10521,#10522,#10523,#10524,
#10525,#10526,#10527,#10528,#10529,#10530,#10531),.UNSPECIFIED.,.T.,.F.,
(4,2,2,2,2,2,2,2,2,2,2,2,2,2,2,2,4),(-0.756843550264884,-0.709537521260487,
-0.662231492256091,-0.614932077477377,-0.567632662698663,-0.520333247919949,
-0.473033833141235,-0.425727804136839,-0.378421775132442,-0.331115746128045,
-0.283809717123649,-0.236510302344935,-0.189210887566221,-0.141911472787507,
-0.0946120580087934,-0.0473060290043967,0.),.UNSPECIFIED.);
#173=B_SPLINE_CURVE_WITH_KNOTS('',3,(#10598,#10599,#10600,#10601,#10602,
#10603,#10604,#10605,#10606,#10607,#10608,#10609,#10610,#10611,#10612,#10613,
#10614,#10615,#10616,#10617,#10618,#10619,#10620,#10621,#10622,#10623,#10624,
#10625,#10626,#10627,#10628,#10629,#10630,#10631),.UNSPECIFIED.,.T.,.F.,
(4,2,2,2,2,2,2,2,2,2,2,2,2,2,2,2,4),(0.,0.0481144001101842,0.0962288002203683,
0.144212038136127,0.192195276051885,0.240178513967643,0.288161751883402,
0.336276151993586,0.38439055210377,0.432504952213954,0.480619352324138,
0.528602590239897,0.576585828155655,0.624569066071413,0.672552303987172,
0.720666704097356,0.76878110420754),.UNSPECIFIED.);
#174=B_SPLINE_CURVE_WITH_KNOTS('',3,(#10634,#10635,#10636,#10637,#10638,
#10639,#10640,#10641,#10642,#10643,#10644,#10645,#10646,#10647,#10648,#10649,
#10650,#10651),.UNSPECIFIED.,.F.,.F.,(4,2,2,2,2,2,2,2,4),(0.192195276051885,
0.240178513967643,0.288161751883402,0.336276151993586,0.38439055210377,
0.432504952213954,0.480619352324138,0.528602590239897,0.576585828155655),
 .UNSPECIFIED.);
#175=B_SPLINE_CURVE_WITH_KNOTS('',3,(#10652,#10653,#10654,#10655,#10656,
#10657,#10658,#10659,#10660,#10661,#10662,#10663,#10664,#10665,#10666,#10667,
#10668,#10669,#10670),.UNSPECIFIED.,.F.,.F.,(4,2,2,2,3,2,2,2,4),(0.576585828155655,
0.624569066071413,0.672552303987172,0.720666704097356,0.76878110420754,
0.816895504317724,0.865009904427908,0.912993142343667,0.960976380259425),
 .UNSPECIFIED.);
#176=B_SPLINE_CURVE_WITH_KNOTS('',3,(#10699,#10700,#10701,#10702,#10703,
#10704,#10705,#10706,#10707,#10708),.UNSPECIFIED.,.F.,.F.,(4,2,2,2,4),(-0.377880095159423,
-0.330643519967439,-0.283406944775455,-0.236173496177583,-0.188940047579712),
 .UNSPECIFIED.);
#177=B_SPLINE_CURVE_WITH_KNOTS('',3,(#10712,#10713,#10714,#10715,#10716,
#10717,#10718,#10719,#10720,#10721),.UNSPECIFIED.,.F.,.F.,(4,2,2,2,4),(0.188940047579712,
0.236173496177583,0.283406944775455,0.330643519967439,0.377880095159423),
 .UNSPECIFIED.);
#178=B_SPLINE_CURVE_WITH_KNOTS('',3,(#10723,#10724,#10725,#10726,#10727,
#10728,#10729,#10730,#10731,#10732,#10733,#10734,#10735,#10736,#10737,#10738,
#10739,#10740,#10741,#10742,#10743,#10744,#10745),.UNSPECIFIED.,.F.,.F.,
(4,2,2,2,2,2,3,2,2,2,4),(-0.276474823920439,-0.236173496177583,-0.188940047579712,
-0.14170659898184,-0.0944731503839682,-0.0472365751919841,0.,0.0472365751919841,
0.0944731503839681,0.14170659898184,0.188940047579712),.UNSPECIFIED.);
#179=B_SPLINE_CURVE_WITH_KNOTS('',3,(#10752,#10753,#10754,#10755,#10756,
#10757,#10758,#10759,#10760,#10761,#10762,#10763,#10764,#10765,#10766,#10767,
#10768,#10769,#10770),.UNSPECIFIED.,.F.,.F.,(4,2,2,2,3,2,2,2,4),(-0.188940047579712,
-0.14170659898184,-0.0944731503839681,-0.0472365751919841,0.,0.0472365751919841,
0.0944731503839682,0.14170659898184,0.188940047579712),.UNSPECIFIED.);
#180=B_SPLINE_CURVE_WITH_KNOTS('',3,(#10799,#10800,#10801,#10802),
 .UNSPECIFIED.,.F.,.F.,(4,4),(0.0419009061515246,0.24114214195851),
 .UNSPECIFIED.);
#181=B_SPLINE_CURVE_WITH_KNOTS('',3,(#10803,#10804,#10805,#10806,#10807,
#10808),.UNSPECIFIED.,.F.,.F.,(4,2,4),(-0.160890299009028,-0.155410119436095,
-0.148763314259543),.UNSPECIFIED.);
#182=B_SPLINE_CURVE_WITH_KNOTS('',3,(#10810,#10811,#10812,#10813,#10814,
#10815),.UNSPECIFIED.,.F.,.F.,(4,2,4),(-0.173042755318085,-0.172254926856018,
-0.160890299013474),.UNSPECIFIED.);
#183=B_SPLINE_CURVE_WITH_KNOTS('',3,(#10816,#10817,#10818,#10819),
 .UNSPECIFIED.,.F.,.F.,(4,4),(0.488884303449535,0.688125539256493),
 .UNSPECIFIED.);
#184=B_SPLINE_CURVE_WITH_KNOTS('',3,(#10845,#10846,#10847,#10848,#10849,
#10850),.UNSPECIFIED.,.F.,.F.,(4,2,4),(0.188940047579712,0.236173496177584,
0.276474823920109),.UNSPECIFIED.);
#185=B_SPLINE_CURVE_WITH_KNOTS('',3,(#10854,#10855,#10856,#10857,#10858,
#10859,#10860,#10861,#10862,#10863,#10864,#10865,#10866,#10867,#10868,#10869,
#10870,#10871),.UNSPECIFIED.,.F.,.F.,(4,2,2,2,2,2,2,2,4),(0.192195276051885,
0.240178513967644,0.288161751883402,0.336276151993586,0.38439055210377,
0.432504952213954,0.480619352324138,0.528602590239897,0.576585828155655),
 .UNSPECIFIED.);
#186=B_SPLINE_CURVE_WITH_KNOTS('',3,(#10872,#10873,#10874,#10875,#10876,
#10877,#10878,#10879,#10880,#10881,#10882,#10883,#10884,#10885,#10886,#10887,
#10888,#10889,#10890),.UNSPECIFIED.,.F.,.F.,(4,2,2,2,3,2,2,2,4),(-0.192195276051885,
-0.144212038136127,-0.0962288002203683,-0.0481144001101841,1.11022302462516E-16,
0.0481144001101843,0.0962288002203684,0.144212038136127,0.192195276051885),
 .UNSPECIFIED.);
#187=B_SPLINE_CURVE_WITH_KNOTS('',3,(#10894,#10895,#10896,#10897,#10898,
#10899,#10900,#10901,#10902,#10903,#10904,#10905,#10906,#10907,#10908,#10909,
#10910,#10911,#10912),.UNSPECIFIED.,.F.,.F.,(4,2,2,2,3,2,2,2,4),(-0.192195276051885,
-0.144212038136127,-0.0962288002203683,-0.0481144001101841,0.,0.0481144001101841,
0.0962288002203683,0.144212038136127,0.192195276051885),.UNSPECIFIED.);
#188=B_SPLINE_CURVE_WITH_KNOTS('',3,(#10913,#10914,#10915,#10916,#10917,
#10918,#10919,#10920,#10921,#10922,#10923,#10924,#10925,#10926,#10927,#10928,
#10929,#10930),.UNSPECIFIED.,.F.,.F.,(4,2,2,2,2,2,2,2,4),(0.192195276051885,
0.240178513967643,0.288161751883402,0.336276151993586,0.38439055210377,
0.432504952213954,0.480619352324138,0.528602590239897,0.576585828155655),
 .UNSPECIFIED.);
#189=B_SPLINE_CURVE_WITH_KNOTS('',3,(#11014,#11015,#11016,#11017,#11018,
#11019,#11020,#11021,#11022,#11023,#11024,#11025,#11026,#11027,#11028,#11029,
#11030,#11031),.UNSPECIFIED.,.F.,.F.,(4,2,2,2,2,2,2,2,4),(-0.576585828155656,
-0.528602590239897,-0.480619352324139,-0.432504952213955,-0.384390552103771,
-0.336276151993587,-0.288161751883402,-0.240178513967644,-0.192195276051885),
 .UNSPECIFIED.);
#190=B_SPLINE_CURVE_WITH_KNOTS('',3,(#11035,#11036,#11037,#11038,#11039,
#11040,#11041,#11042,#11043,#11044,#11045,#11046,#11047,#11048,#11049,#11050,
#11051,#11052),.UNSPECIFIED.,.F.,.F.,(4,2,2,2,2,2,2,2,4),(0.192195276051885,
0.240178513967643,0.288161751883402,0.336276151993586,0.38439055210377,
0.432504952213954,0.480619352324138,0.528602590239897,0.576585828155655),
 .UNSPECIFIED.);
#191=B_SPLINE_CURVE_WITH_KNOTS('',3,(#11054,#11055,#11056,#11057,#11058,
#11059,#11060,#11061,#11062,#11063,#11064,#11065,#11066,#11067,#11068,#11069,
#11070,#11071,#11072),.UNSPECIFIED.,.F.,.F.,(4,2,2,2,3,2,2,2,4),(0.576585828155655,
0.624569066071413,0.672552303987172,0.720666704097356,0.76878110420754,
0.816895504317724,0.865009904427908,0.912993142343667,0.960976380259425),
 .UNSPECIFIED.);
#192=B_SPLINE_CURVE_WITH_KNOTS('',3,(#11073,#11074,#11075,#11076,#11077,
#11078,#11079,#11080,#11081,#11082,#11083,#11084,#11085,#11086,#11087,#11088,
#11089,#11090,#11091),.UNSPECIFIED.,.F.,.F.,(4,2,2,2,3,2,2,2,4),(-0.192195276051885,
-0.144212038136127,-0.0962288002203689,-0.0481144001101845,0.,0.0481144001101841,
0.0962288002203682,0.144212038136126,0.192195276051885),.UNSPECIFIED.);
#193=B_SPLINE_CURVE_WITH_KNOTS('',3,(#11094,#11095,#11096,#11097,#11098,
#11099,#11100,#11101,#11102,#11103,#11104,#11105,#11106,#11107,#11108,#11109,
#11110,#11111,#11112),.UNSPECIFIED.,.F.,.F.,(4,2,2,2,3,2,2,2,4),(0.576585828155656,
0.624569066071414,0.672552303987172,0.720666704097356,0.76878110420754,
0.816895504317725,0.865009904427909,0.912993142343667,0.960976380259426),
 .UNSPECIFIED.);
#194=B_SPLINE_CURVE_WITH_KNOTS('',3,(#11113,#11114,#11115,#11116,#11117,
#11118,#11119,#11120,#11121,#11122,#11123,#11124,#11125,#11126,#11127,#11128,
#11129,#11130),.UNSPECIFIED.,.F.,.F.,(4,2,2,2,2,2,2,2,4),(0.960976380259426,
1.00895961817518,1.05694285609094,1.10505725620113,1.15317165631131,1.2012860564215,
1.24940045653168,1.29738369444744,1.3453669323632),.UNSPECIFIED.);
#195=B_SPLINE_CURVE_WITH_KNOTS('',3,(#11132,#11133,#11134,#11135,#11136,
#11137,#11138,#11139,#11140,#11141,#11142,#11143,#11144,#11145,#11146,#11147,
#11148,#11149,#11150,#11151,#11152,#11153,#11154,#11155,#11156,#11157,#11158,
#11159,#11160,#11161,#11162,#11163,#11164,#11165),.UNSPECIFIED.,.T.,.F.,
(4,2,2,2,2,2,2,2,2,2,2,2,2,2,2,2,4),(0.,0.0481144001101842,0.0962288002203683,
0.144212038136127,0.192195276051885,0.240178513967643,0.288161751883402,
0.336276151993586,0.38439055210377,0.432504952213954,0.480619352324138,
0.528602590239897,0.576585828155655,0.624569066071413,0.672552303987172,
0.720666704097356,0.76878110420754),.UNSPECIFIED.);
#196=B_SPLINE_CURVE_WITH_KNOTS('',3,(#11224,#11225,#11226,#11227,#11228,
#11229,#11230,#11231,#11232,#11233,#11234,#11235,#11236,#11237,#11238,#11239,
#11240,#11241),.UNSPECIFIED.,.F.,.F.,(4,2,2,2,2,2,2,2,4),(-1.05841496918539,
-0.992261360989225,-0.926107752793056,-0.859959489841051,-0.793811226889045,
-0.72766296393704,-0.661514700985034,-0.595361092788865,-0.529207484592697),
 .UNSPECIFIED.);
#197=B_SPLINE_CURVE_WITH_KNOTS('',3,(#11242,#11243,#11244,#11245,#11246,
#11247,#11248,#11249,#11250,#11251,#11252,#11253,#11254,#11255,#11256,#11257,
#11258,#11259),.UNSPECIFIED.,.F.,.F.,(4,2,2,2,2,2,2,2,4),(-0.529207484592697,
-0.463053876396528,-0.39690026820036,-0.330752005248354,-0.264603742296348,
-0.198455479344343,-0.132307216392337,-0.0661536081961685,0.),
 .UNSPECIFIED.);
#198=B_SPLINE_CURVE_WITH_KNOTS('',3,(#11269,#11270,#11271,#11272,#11273,
#11274,#11275,#11276,#11277,#11278,#11279,#11280,#11281,#11282,#11283,#11284,
#11285,#11286),.UNSPECIFIED.,.F.,.F.,(4,2,2,2,2,2,2,2,4),(0.,0.0756896464070345,
0.151379292814069,0.227058356460011,0.302737420105953,0.378416483751896,
0.454095547397838,0.529785193804872,0.605474840211907),.UNSPECIFIED.);
#199=B_SPLINE_CURVE_WITH_KNOTS('',3,(#11287,#11288,#11289,#11290,#11291,
#11292,#11293,#11294,#11295,#11296,#11297,#11298,#11299,#11300,#11301,#11302,
#11303,#11304),.UNSPECIFIED.,.F.,.F.,(4,2,2,2,2,2,2,2,4),(0.605474840211907,
0.681164486618941,0.756854133025976,0.832533196671918,0.90821226031786,
0.983891323963802,1.05957038760974,1.13526003401678,1.21094968042381),
 .UNSPECIFIED.);
#200=B_SPLINE_CURVE_WITH_KNOTS('',3,(#11355,#11356,#11357,#11358,#11359,
#11360,#11361,#11362,#11363,#11364,#11365,#11366,#11367,#11368,#11369,#11370,
#11371,#11372,#11373,#11374,#11375,#11376,#11377,#11378,#11379,#11380,#11381,
#11382,#11383,#11384,#11385,#11386,#11387,#11388),.UNSPECIFIED.,.T.,.F.,
(4,2,2,2,2,2,2,2,2,2,2,2,2,2,2,2,4),(-1.20857841771805,-1.13304053166828,
-1.05750264561851,-0.981968229453524,-0.906433813288534,-0.830899397123545,
-0.755364980958556,-0.679827094908789,-0.604289208859023,-0.528751322809257,
-0.45321343675949,-0.377679020594501,-0.302144604429511,-0.226610188264522,
-0.151075772099533,-0.0755378860497663,0.),.UNSPECIFIED.);
#201=B_SPLINE_CURVE_WITH_KNOTS('',3,(#11395,#11396,#11397,#11398),
 .UNSPECIFIED.,.F.,.F.,(4,4),(2.52799303913365E-15,0.312557295914921),
 .UNSPECIFIED.);
#202=B_SPLINE_CURVE_WITH_KNOTS('',3,(#11399,#11400,#11401,#11402),
 .UNSPECIFIED.,.F.,.F.,(4,4),(0.616643793973297,0.929201089887433),
 .UNSPECIFIED.);
#203=B_SPLINE_CURVE_WITH_KNOTS('',3,(#11526,#11527,#11528,#11529,#11530,
#11531,#11532,#11533,#11534,#11535,#11536,#11537,#11538,#11539,#11540,#11541,
#11542,#11543,#11544,#11545,#11546,#11547),.UNSPECIFIED.,.F.,.F.,(4,2,2,
2,2,2,2,2,2,2,4),(-0.102916914552731,-0.0960165368188152,-0.0889835057043814,
-0.0739989051443188,-0.0615887125232106,-0.0518493032905911,-0.0421259736973909,
-0.0296860378067567,-0.0142968246061035,-0.00712380381615376,-1.60735926204118E-5),
 .UNSPECIFIED.);
#204=B_SPLINE_CURVE_WITH_KNOTS('',3,(#11548,#11549,#11550,#11551,#11552,
#11553,#11554,#11555,#11556,#11557,#11558,#11559,#11560,#11561,#11562,#11563,
#11564,#11565,#11566,#11567,#11568,#11569),.UNSPECIFIED.,.F.,.F.,(4,2,2,
2,2,2,2,2,2,2,4),(-0.10788302753294,-0.100819295498672,-0.0936081097542318,
-0.077747080264816,-0.0645335298256269,-0.0542154745376808,-0.0438805066497465,
-0.0307065427009455,-0.0148008794241195,-0.00733029393624065,-1.25860813603491E-6),
 .UNSPECIFIED.);
#205=B_SPLINE_CURVE_WITH_KNOTS('',3,(#11921,#11922,#11923,#11924,#11925,
#11926,#11927,#11928,#11929,#11930,#11931,#11932,#11933,#11934,#11935,#11936,
#11937,#11938,#11939,#11940,#11941,#11942,#11943,#11944,#11945,#11946,#11947,
#11948,#11949,#11950,#11951,#11952,#11953,#11954,#11955,#11956,#11957,#11958,
#11959,#11960,#11961,#11962,#11963,#11964,#11965,#11966,#11967,#11968,#11969,
#11970,#11971,#11972,#11973,#11974,#11975,#11976,#11977,#11978,#11979,#11980,
#11981,#11982,#11983,#11984,#11985,#11986,#11987,#11988,#11989,#11990,#11991,
#11992,#11993,#11994,#11995,#11996,#11997,#11998,#11999,#12000,#12001,#12002,
#12003,#12004,#12005,#12006,#12007,#12008,#12009,#12010,#12011,#12012,#12013,
#12014,#12015,#12016,#12017,#12018,#12019,#12020,#12021,#12022,#12023,#12024,
#12025,#12026,#12027,#12028,#12029,#12030,#12031,#12032,#12033,#12034,#12035,
#12036,#12037,#12038,#12039,#12040,#12041,#12042,#12043,#12044,#12045,#12046,
#12047,#12048,#12049,#12050,#12051,#12052,#12053,#12054,#12055,#12056,#12057,
#12058,#12059,#12060,#12061,#12062,#12063,#12064,#12065,#12066,#12067,#12068,
#12069,#12070,#12071,#12072,#12073,#12074,#12075,#12076,#12077,#12078,#12079,
#12080,#12081,#12082,#12083,#12084,#12085,#12086,#12087,#12088,#12089,#12090,
#12091,#12092,#12093,#12094,#12095,#12096,#12097,#12098,#12099,#12100,#12101,
#12102,#12103,#12104,#12105,#12106,#12107,#12108,#12109,#12110,#12111,#12112,
#12113,#12114,#12115,#12116,#12117,#12118,#12119,#12120,#12121,#12122,#12123,
#12124,#12125,#12126,#12127,#12128,#12129,#12130,#12131,#12132,#12133,#12134,
#12135,#12136,#12137,#12138,#12139,#12140,#12141,#12142,#12143,#12144,#12145,
#12146,#12147,#12148,#12149,#12150,#12151,#12152,#12153,#12154,#12155,#12156,
#12157,#12158,#12159,#12160,#12161,#12162,#12163,#12164,#12165,#12166,#12167,
#12168,#12169,#12170,#12171,#12172,#12173,#12174,#12175,#12176,#12177,#12178,
#12179,#12180,#12181,#12182,#12183,#12184,#12185,#12186,#12187,#12188,#12189,
#12190,#12191,#12192,#12193,#12194,#12195,#12196,#12197,#12198,#12199,#12200,
#12201,#12202,#12203,#12204,#12205,#12206,#12207,#12208,#12209,#12210,#12211,
#12212,#12213,#12214,#12215,#12216,#12217,#12218,#12219,#12220,#12221,#12222,
#12223,#12224,#12225,#12226,#12227,#12228,#12229,#12230,#12231,#12232,#12233,
#12234,#12235,#12236,#12237,#12238,#12239,#12240,#12241,#12242,#12243,#12244,
#12245,#12246,#12247,#12248,#12249,#12250,#12251,#12252,#12253,#12254,#12255,
#12256,#12257,#12258,#12259,#12260,#12261,#12262,#12263,#12264,#12265,#12266,
#12267,#12268,#12269,#12270,#12271,#12272,#12273,#12274,#12275,#12276,#12277,
#12278,#12279,#12280,#12281,#12282,#12283,#12284,#12285,#12286,#12287,#12288,
#12289,#12290,#12291,#12292,#12293,#12294,#12295,#12296,#12297,#12298,#12299,
#12300,#12301,#12302,#12303,#12304,#12305,#12306,#12307,#12308,#12309,#12310,
#12311,#12312,#12313,#12314,#12315,#12316,#12317,#12318,#12319,#12320,#12321,
#12322,#12323,#12324,#12325,#12326,#12327,#12328,#12329,#12330,#12331,#12332,
#12333,#12334,#12335,#12336,#12337,#12338,#12339,#12340,#12341,#12342,#12343,
#12344,#12345,#12346,#12347,#12348,#12349,#12350,#12351,#12352,#12353,#12354,
#12355,#12356,#12357,#12358,#12359,#12360,#12361,#12362,#12363,#12364,#12365,
#12366,#12367,#12368,#12369,#12370,#12371,#12372,#12373,#12374,#12375,#12376,
#12377,#12378,#12379,#12380,#12381,#12382,#12383,#12384,#12385,#12386,#12387,
#12388,#12389,#12390,#12391,#12392,#12393,#12394,#12395,#12396,#12397,#12398,
#12399,#12400,#12401,#12402,#12403,#12404,#12405,#12406,#12407,#12408,#12409,
#12410,#12411,#12412,#12413,#12414,#12415,#12416,#12417,#12418,#12419,#12420,
#12421,#12422,#12423,#12424,#12425,#12426,#12427,#12428,#12429,#12430,#12431,
#12432,#12433,#12434,#12435,#12436,#12437,#12438,#12439,#12440,#12441,#12442,
#12443,#12444,#12445,#12446,#12447,#12448,#12449,#12450,#12451,#12452,#12453,
#12454,#12455,#12456,#12457,#12458,#12459,#12460,#12461,#12462,#12463,#12464,
#12465,#12466,#12467,#12468,#12469,#12470,#12471,#12472,#12473),
 .UNSPECIFIED.,.F.,.F.,(4,3,3,3,3,3,3,3,3,3,3,3,3,3,3,3,3,3,3,3,3,3,3,3,
3,3,3,3,3,3,3,3,3,3,3,3,3,3,3,3,3,3,3,3,3,3,3,3,3,3,3,3,3,3,3,3,3,3,3,3,
3,3,3,3,3,3,3,3,3,3,3,3,3,3,3,3,3,3,3,3,3,3,3,3,3,3,3,3,3,3,3,3,3,3,3,3,
3,3,3,3,3,3,3,3,3,3,3,3,3,3,3,3,3,3,3,3,3,3,3,3,3,3,3,3,3,3,3,3,3,3,3,3,
3,3,3,3,3,3,3,3,3,3,3,3,3,3,3,3,3,3,3,3,3,3,3,3,3,3,3,3,3,3,3,3,3,3,3,3,
3,3,3,3,3,3,3,3,3,3,3,3,3,3,3,3,4),(0.,0.00625925877618659,0.012498777633829,
0.01694915254237,0.0234628389430874,0.0301365197565823,0.03389830508475,
0.0399395455000561,0.0449988746104484,0.05084745762712,0.0573237266639631,
0.0638987543535039,0.06779661016949,0.0736716349306864,0.0774993881424463,
0.0833663385077181,0.08474576271186,0.091167331299509,0.097628739000386,
0.1016949152542,0.107513390502625,0.110000096381761,0.115819871711873,0.1186440677966,
0.12510195465327,0.131545205429102,0.135593220339,0.141479707111754,0.142500758971052,
0.148398207638992,0.1525423728814,0.159137176794001,0.165656536879295,0.1694915254237,
0.175001153770124,0.181104985312333,0.1864406779661,0.193291692194109,0.199994170967044,
0.2033898305085,0.207501144893393,0.213996704784992,0.2203389830508,0.227648989561867,
0.234707372019173,0.2372881355932,0.240000783824304,0.247222805643196,0.2542372881356,
0.2627118644068,0.270472303966788,0.271186440678,0.272500297957407,0.281244760606251,
0.2881355932203,0.297798413321956,0.304999991245754,0.3050847457627,0.314508174872632,
0.3220338983051,0.330512021731323,0.337499649903537,0.3389830508475,0.346615949971345,
0.354646702577775,0.3559322033898,0.363033438865616,0.369999163432914,0.3728813559322,
0.37985332543126,0.387078943207013,0.3898305084746,0.396262716777247,0.402498837141279,
0.4067796610169,0.413421019419821,0.420230556868151,0.4237288135593,0.429797841794845,
0.434998879663644,0.4406779661017,0.447154148986824,0.453734297968348,0.4576271186441,
0.46350827908289,0.467499317471382,0.47337093009509,0.4745762711864,0.48099518354306,
0.487461530539164,0.4915254237288,0.497345526991414,0.500000003734255,0.505820187494862,
0.5084745762712,0.514924727843856,0.521366864166133,0.5254237288136,0.531295850595029,
0.532500689595544,0.538382527082556,0.5423728813559,0.54894525402918,0.555450031435636,
0.5593220338983,0.565001126342026,0.571071570720213,0.5762711864407,0.583082695457437,
0.589755631698227,0.5932203389831,0.597501167527674,0.603935922491351,0.6101694915254,
0.617407999264796,0.624410071113853,0.6271186440678,0.630000840110392,0.637106843597801,
0.6440677966102,0.65254237288135,0.660180609988071,0.6610169491525,0.662500353088126,
0.670988906543055,0.6779661016949,0.687400217121739,0.6949152542373,0.695000011705008,
0.704653651272696,0.7118644067797,0.720597517779026,0.727499705010129,0.728813559322,
0.736568079962082,0.744745446872398,0.7457627118644,0.752979538682311,0.759999219617496,
0.7627118644068,0.769740858446909,0.777036628437343,0.7796610169492,0.786153842810917,
0.792498859618453,0.7966101694915,0.803280942492757,0.810128713700182,0.8135593220339,
0.81966162847591,0.824998852078597,0.8305084745763,0.836998731347478,0.843600194647583,
0.8474576271186,0.853354320256163,0.85749924799678,0.863385148965961,0.864406779661,
0.870826069225487,0.877299244450954,0.8813559322034,0.887175557231592,0.889999911082328,
0.895818397253527,0.8983050847458,0.904749271770384,0.911193161122928,0.9152542372881,
0.921121621454876,0.922500619004354,0.928376243104498,0.9322033898305,0.938769848536967,
0.945274226985483,0.9491525423729,0.955001131578282,0.961043720040324,0.9661016949153,
0.972776378140019,0.979322863868025,0.9830508474576,0.987501227214033,0.993762571705349,
1.),.UNSPECIFIED.);
#206=B_SPLINE_CURVE_WITH_KNOTS('',3,(#12475,#12476,#12477,#12478,#12479,
#12480,#12481,#12482,#12483,#12484,#12485,#12486,#12487,#12488,#12489,#12490,
#12491,#12492,#12493,#12494,#12495,#12496,#12497,#12498,#12499,#12500,#12501,
#12502,#12503,#12504,#12505,#12506,#12507,#12508,#12509,#12510,#12511,#12512,
#12513,#12514,#12515,#12516,#12517,#12518,#12519,#12520,#12521,#12522,#12523,
#12524,#12525,#12526,#12527,#12528,#12529),.UNSPECIFIED.,.F.,.F.,(4,3,3,
3,3,3,3,3,3,3,3,3,3,3,3,3,3,3,4),(2.3090748468048E-7,4.45838606717901E-5,
0.103040149515435,0.193721878728962,0.25,0.251116964176227,0.330254232791472,
0.414362786406979,0.487704402387173,0.498471340022485,0.5,0.590018211493824,
0.65062380043533,0.733876213547321,0.75,0.804169141594039,0.887250644440787,
0.959806362373788,1.),.UNSPECIFIED.);
#207=B_SPLINE_CURVE_WITH_KNOTS('',3,(#12530,#12531,#12532,#12533,#12534,
#12535,#12536,#12537,#12538,#12539,#12540,#12541,#12542,#12543,#12544,#12545,
#12546,#12547,#12548,#12549,#12550,#12551,#12552,#12553,#12554,#12555,#12556,
#12557,#12558,#12559,#12560,#12561,#12562,#12563,#12564,#12565,#12566,#12567,
#12568,#12569,#12570,#12571,#12572,#12573,#12574,#12575,#12576,#12577,#12578,
#12579,#12580,#12581,#12582,#12583,#12584,#12585,#12586,#12587,#12588,#12589,
#12590,#12591,#12592,#12593,#12594,#12595,#12596,#12597,#12598,#12599,#12600,
#12601,#12602,#12603,#12604,#12605,#12606,#12607,#12608,#12609,#12610,#12611,
#12612,#12613,#12614,#12615,#12616,#12617,#12618,#12619,#12620,#12621,#12622,
#12623,#12624,#12625,#12626,#12627,#12628,#12629,#12630,#12631,#12632,#12633,
#12634,#12635,#12636,#12637,#12638,#12639,#12640,#12641,#12642,#12643,#12644,
#12645,#12646,#12647,#12648,#12649,#12650,#12651,#12652,#12653,#12654,#12655,
#12656,#12657,#12658,#12659,#12660,#12661,#12662,#12663,#12664,#12665,#12666,
#12667,#12668,#12669,#12670,#12671,#12672,#12673,#12674,#12675,#12676,#12677,
#12678,#12679,#12680,#12681,#12682,#12683,#12684,#12685,#12686,#12687,#12688,
#12689,#12690,#12691,#12692,#12693,#12694,#12695,#12696,#12697,#12698,#12699,
#12700,#12701,#12702,#12703,#12704,#12705,#12706,#12707,#12708,#12709,#12710,
#12711,#12712,#12713,#12714,#12715,#12716,#12717,#12718,#12719,#12720,#12721,
#12722,#12723,#12724,#12725,#12726,#12727,#12728,#12729,#12730,#12731,#12732,
#12733,#12734,#12735,#12736,#12737,#12738,#12739,#12740,#12741,#12742,#12743,
#12744,#12745,#12746,#12747,#12748,#12749,#12750,#12751,#12752,#12753,#12754,
#12755,#12756,#12757,#12758,#12759,#12760,#12761,#12762,#12763,#12764,#12765,
#12766,#12767,#12768,#12769,#12770,#12771,#12772,#12773,#12774,#12775,#12776,
#12777,#12778,#12779,#12780,#12781,#12782,#12783,#12784,#12785,#12786,#12787,
#12788,#12789,#12790,#12791,#12792,#12793,#12794,#12795,#12796,#12797,#12798,
#12799,#12800,#12801,#12802,#12803,#12804,#12805,#12806,#12807,#12808,#12809,
#12810,#12811,#12812,#12813,#12814,#12815,#12816,#12817,#12818,#12819,#12820,
#12821,#12822,#12823,#12824,#12825,#12826,#12827,#12828,#12829,#12830,#12831,
#12832,#12833,#12834,#12835,#12836,#12837,#12838,#12839,#12840,#12841,#12842,
#12843,#12844,#12845,#12846,#12847,#12848,#12849,#12850,#12851,#12852,#12853,
#12854,#12855,#12856,#12857,#12858,#12859,#12860,#12861,#12862,#12863,#12864,
#12865,#12866,#12867,#12868,#12869,#12870,#12871,#12872,#12873,#12874,#12875,
#12876,#12877,#12878,#12879,#12880,#12881,#12882,#12883,#12884,#12885,#12886,
#12887,#12888,#12889,#12890,#12891,#12892,#12893,#12894,#12895,#12896,#12897,
#12898,#12899,#12900,#12901,#12902,#12903,#12904,#12905,#12906,#12907,#12908,
#12909,#12910,#12911,#12912,#12913,#12914,#12915,#12916,#12917,#12918,#12919,
#12920,#12921,#12922,#12923,#12924,#12925,#12926,#12927,#12928,#12929,#12930,
#12931,#12932,#12933,#12934,#12935,#12936,#12937,#12938,#12939,#12940,#12941,
#12942,#12943,#12944,#12945,#12946,#12947,#12948,#12949,#12950,#12951,#12952,
#12953,#12954,#12955,#12956,#12957,#12958,#12959,#12960,#12961,#12962,#12963,
#12964,#12965,#12966,#12967,#12968,#12969,#12970,#12971,#12972,#12973,#12974,
#12975,#12976,#12977,#12978,#12979,#12980,#12981,#12982,#12983,#12984,#12985,
#12986,#12987,#12988,#12989,#12990,#12991,#12992,#12993,#12994,#12995,#12996,
#12997,#12998,#12999,#13000,#13001,#13002,#13003,#13004,#13005,#13006,#13007,
#13008,#13009,#13010,#13011,#13012,#13013,#13014,#13015,#13016,#13017,#13018,
#13019,#13020,#13021,#13022,#13023,#13024,#13025,#13026,#13027,#13028,#13029,
#13030,#13031,#13032,#13033,#13034,#13035,#13036,#13037,#13038,#13039,#13040,
#13041,#13042,#13043,#13044,#13045,#13046),.UNSPECIFIED.,.F.,.F.,(4,3,3,
3,3,3,3,3,3,3,3,3,3,3,3,3,3,3,3,3,3,3,3,3,3,3,3,3,3,3,3,3,3,3,3,3,3,3,3,
3,3,3,3,3,3,3,3,3,3,3,3,3,3,3,3,3,3,3,3,3,3,3,3,3,3,3,3,3,3,3,3,3,3,3,3,
3,3,3,3,3,3,3,3,3,3,3,3,3,3,3,3,3,3,3,3,3,3,3,3,3,3,3,3,3,3,3,3,3,3,3,3,
3,3,3,3,3,3,3,3,3,3,3,3,3,3,3,3,3,3,3,3,3,3,3,3,3,3,3,3,3,3,3,3,3,3,3,3,
3,3,3,3,3,3,3,3,3,3,3,3,3,3,3,3,3,3,3,3,3,3,3,3,3,4),(0.,0.00661684428018137,
0.0124983817048157,0.01818181818182,0.0250973632804601,0.0321069440395133,
0.03636363636364,0.0426727072895669,0.0450002377175405,0.0513095386321912,
0.05454545454545,0.0617456270204197,0.0688539157013956,0.07272727272727,
0.0775015374916661,0.0844748541646262,0.09090909090909,0.099999999999995,
0.108428998891845,0.1090909090909,0.110000217048989,0.12078325484281,0.1272727272727,
0.135245023027212,0.142498954904298,0.1454545454545,0.152858323610583,0.160506895105771,
0.1636363636364,0.170111029696646,0.174998755495631,0.181458997908831,0.1818181818182,
0.188790646856768,0.195802632099578,0.2,0.206382022349692,0.207500940523936,
0.213892441612431,0.2181818181818,0.225620518782517,0.232894897619836,0.2363636363636,
0.240001295617423,0.24749297412486,0.2545454545455,0.264726456123787,0.272499960749247,
0.2727272727273,0.282186815835694,0.2909090909091,0.298158858068406,0.30499857495095,
0.3090909090909,0.316250190246083,0.323581911184479,0.3272727272727,0.33362603963409,
0.337499304115395,0.343846043279279,0.3454545454545,0.352469372648584,0.359471200512104,
0.3636363636364,0.370001396088217,0.376550684913404,0.3818181818182,0.389651332870855,
0.397226018556947,0.4,0.402500854077189,0.410898586807204,0.4181818181818,
0.428299197899163,0.434999622589465,0.4363636363636,0.444446016034832,0.452935768204114,
0.4545454545455,0.461363105296409,0.467498436350891,0.4727272727273,0.479753855421816,
0.486893984305155,0.4909090909091,0.497221599841649,0.500000000005468,0.506312508953864,
0.5090909090909,0.51621847416553,0.523276761335571,0.5272727272727,0.532501563654628,
0.539319218740823,0.5454545454545,0.553958909635691,0.562058015370272,0.5636363636364,
0.565000377410551,0.575117784621314,0.5818181818182,0.590215898849764,0.597499145923507,
0.6,0.607544531271774,0.615369919544731,0.6181818181818,0.624731104355087,
0.629998603919711,0.6363636363636,0.643337807116345,0.65037226491035,0.6545454545455,
0.660892194670005,0.662500695894973,0.6688540092563,0.6727272727273,0.680054450651049,
0.687247439083709,0.6909090909091,0.695001425052158,0.702251199224186,0.7090909090909,
0.718550473994048,0.7272727272727,0.727500039250745,0.737681014960217,0.7454545454545,
0.75294621533796,0.759998704384844,0.7636363636364,0.770877063207263,0.778316868345802,
0.7818181818182,0.78820968148288,0.792499059485903,0.798881080459228,0.8,
0.806989821379187,0.813987898953542,0.8181818181818,0.8246420626511,0.825001244513147,
0.831475912696751,0.8363636363636,0.844016416669735,0.851452485846813,0.8545454545455,
0.857501045096921,0.865473353019941,0.8727272727273,0.883510301615267,0.889999782950977,
0.8909090909091,0.899338076324425,0.908253206519462,0.9090909090909,0.916064220506329,
0.922498462512828,0.9272727272727,0.934348434679549,0.941558334052561,0.9454545454545,
0.951763846001661,0.954999762293423,0.961308832885248,0.9636363636364,0.970630377326059,
0.977577339610233,0.9818181818182,0.987501618301725,0.994118465771046,1.),
 .UNSPECIFIED.);
#208=B_SPLINE_CURVE_WITH_KNOTS('',3,(#13292,#13293,#13294,#13295,#13296,
#13297,#13298,#13299,#13300,#13301,#13302,#13303,#13304,#13305,#13306,#13307,
#13308,#13309,#13310,#13311,#13312,#13313,#13314,#13315,#13316,#13317,#13318,
#13319,#13320,#13321,#13322,#13323,#13324,#13325,#13326,#13327,#13328,#13329,
#13330,#13331,#13332,#13333,#13334),.UNSPECIFIED.,.F.,.F.,(4,3,3,3,3,3,
3,3,3,3,3,3,3,3,4),(0.,0.0875545420214221,0.172845777591114,0.25,0.335847439737665,
0.429706536547853,0.5,0.501528659336918,0.577112096273498,0.657242820384804,
0.735419949981763,0.75,0.839853036636981,0.941009610342587,1.),
 .UNSPECIFIED.);
#209=B_SPLINE_CURVE_WITH_KNOTS('',3,(#13581,#13582,#13583,#13584,#13585,
#13586,#13587,#13588,#13589,#13590,#13591,#13592,#13593,#13594,#13595,#13596,
#13597,#13598,#13599,#13600,#13601,#13602,#13603,#13604,#13605,#13606,#13607,
#13608,#13609,#13610,#13611,#13612,#13613,#13614,#13615,#13616,#13617,#13618,
#13619,#13620,#13621,#13622,#13623,#13624,#13625,#13626,#13627,#13628,#13629,
#13630,#13631,#13632,#13633,#13634,#13635,#13636,#13637,#13638,#13639,#13640,
#13641,#13642,#13643,#13644,#13645,#13646,#13647,#13648,#13649,#13650,#13651,
#13652,#13653,#13654,#13655,#13656,#13657,#13658,#13659,#13660,#13661,#13662,
#13663,#13664,#13665,#13666,#13667,#13668,#13669,#13670,#13671,#13672,#13673,
#13674,#13675,#13676,#13677,#13678,#13679,#13680,#13681,#13682,#13683,#13684,
#13685,#13686,#13687,#13688,#13689,#13690,#13691,#13692,#13693,#13694,#13695,
#13696,#13697,#13698,#13699,#13700,#13701,#13702,#13703,#13704,#13705,#13706,
#13707,#13708,#13709,#13710,#13711,#13712,#13713,#13714,#13715,#13716,#13717,
#13718,#13719,#13720,#13721,#13722,#13723,#13724,#13725,#13726,#13727,#13728,
#13729,#13730,#13731,#13732,#13733,#13734,#13735,#13736,#13737,#13738,#13739,
#13740,#13741,#13742,#13743,#13744,#13745,#13746,#13747,#13748,#13749,#13750,
#13751,#13752,#13753,#13754,#13755,#13756,#13757,#13758,#13759,#13760,#13761,
#13762,#13763,#13764,#13765,#13766,#13767,#13768,#13769,#13770,#13771,#13772,
#13773,#13774,#13775,#13776,#13777,#13778,#13779,#13780,#13781,#13782,#13783,
#13784,#13785,#13786,#13787,#13788,#13789,#13790,#13791,#13792,#13793,#13794,
#13795,#13796,#13797,#13798,#13799,#13800,#13801,#13802,#13803,#13804,#13805,
#13806,#13807,#13808,#13809,#13810,#13811,#13812,#13813,#13814,#13815,#13816,
#13817,#13818,#13819,#13820,#13821,#13822,#13823,#13824,#13825,#13826,#13827,
#13828,#13829,#13830,#13831,#13832,#13833,#13834,#13835,#13836,#13837,#13838,
#13839,#13840,#13841,#13842,#13843,#13844,#13845,#13846,#13847,#13848,#13849,
#13850,#13851,#13852,#13853,#13854,#13855,#13856,#13857,#13858,#13859,#13860,
#13861,#13862,#13863,#13864,#13865,#13866,#13867,#13868,#13869,#13870,#13871,
#13872,#13873,#13874,#13875,#13876,#13877,#13878,#13879,#13880,#13881,#13882,
#13883,#13884,#13885,#13886,#13887,#13888,#13889,#13890,#13891,#13892,#13893,
#13894,#13895,#13896,#13897,#13898,#13899,#13900,#13901,#13902,#13903,#13904,
#13905,#13906,#13907,#13908,#13909,#13910,#13911,#13912,#13913,#13914,#13915,
#13916,#13917,#13918,#13919,#13920,#13921,#13922,#13923,#13924,#13925,#13926,
#13927,#13928,#13929,#13930,#13931,#13932,#13933,#13934,#13935,#13936,#13937,
#13938,#13939,#13940,#13941,#13942,#13943,#13944,#13945,#13946,#13947,#13948,
#13949,#13950,#13951,#13952,#13953,#13954,#13955,#13956,#13957,#13958,#13959,
#13960,#13961,#13962,#13963,#13964,#13965,#13966,#13967,#13968,#13969,#13970,
#13971,#13972,#13973,#13974,#13975,#13976,#13977,#13978,#13979,#13980,#13981,
#13982,#13983,#13984,#13985,#13986,#13987,#13988,#13989,#13990,#13991,#13992,
#13993,#13994,#13995,#13996,#13997,#13998,#13999,#14000,#14001,#14002,#14003,
#14004,#14005,#14006,#14007,#14008,#14009,#14010,#14011,#14012,#14013,#14014,
#14015,#14016,#14017,#14018,#14019,#14020,#14021,#14022,#14023,#14024,#14025,
#14026,#14027,#14028,#14029,#14030,#14031,#14032,#14033,#14034,#14035,#14036,
#14037,#14038,#14039,#14040,#14041,#14042,#14043,#14044,#14045,#14046,#14047,
#14048,#14049,#14050,#14051,#14052,#14053,#14054,#14055,#14056,#14057,#14058,
#14059,#14060,#14061,#14062,#14063,#14064,#14065,#14066,#14067,#14068,#14069,
#14070,#14071,#14072,#14073,#14074,#14075,#14076,#14077,#14078,#14079,#14080,
#14081,#14082,#14083,#14084,#14085,#14086,#14087,#14088,#14089,#14090,#14091,
#14092,#14093,#14094,#14095,#14096,#14097),.UNSPECIFIED.,.F.,.F.,(4,3,3,
3,3,3,3,3,3,3,3,3,3,3,3,3,3,3,3,3,3,3,3,3,3,3,3,3,3,3,3,3,3,3,3,3,3,3,3,
3,3,3,3,3,3,3,3,3,3,3,3,3,3,3,3,3,3,3,3,3,3,3,3,3,3,3,3,3,3,3,3,3,3,3,3,
3,3,3,3,3,3,3,3,3,3,3,3,3,3,3,3,3,3,3,3,3,3,3,3,3,3,3,3,3,3,3,3,3,3,3,3,
3,3,3,3,3,3,3,3,3,3,3,3,3,3,3,3,3,3,3,3,3,3,3,3,3,3,3,3,3,3,3,3,3,3,3,3,
3,3,3,3,3,3,3,3,3,3,3,3,3,3,3,3,3,3,3,3,3,3,3,3,3,4),(0.,0.00661684587302782,
0.0124983817015463,0.01818181818182,0.0250973637783485,0.0321069452291795,
0.03636363636364,0.0426727071234974,0.0450002377120509,0.0513095384439047,
0.05454545454545,0.0617456257734155,0.0688539134555847,0.07272727272727,
0.0775015374894108,0.084474851540618,0.09090909090909,0.099999999999995,
0.108428992128763,0.1090909090909,0.110000217049007,0.120783250406177,0.1272727272727,
0.135245029127456,0.14249895490368,0.1454545454545,0.152858325981983,0.160506900311987,
0.1636363636364,0.170111030760943,0.174998755491235,0.181458998931494,0.1818181818182,
0.188790646918572,0.195802632397153,0.2,0.20638202166108,0.207500940519021,
0.213892440897584,0.2181818181818,0.225620516663454,0.232894893756121,0.2363636363636,
0.240001295616291,0.247492969823263,0.2545454545455,0.264726443160001,0.272499960749249,
0.2727272727273,0.282186826709124,0.2909090909091,0.298158861584354,0.304998574949388,
0.3090909090909,0.316250191676838,0.323581914343074,0.3272727272727,0.333626040135667,
0.337499304110203,0.343846043754309,0.3454545454545,0.352469372214191,0.359471199824338,
0.3636363636364,0.37000139608426,0.376550683586942,0.3818181818182,0.389651329369765,
0.397226012189459,0.4,0.402500854076844,0.41089857897861,0.4181818181818,
0.428299211683496,0.434999622589454,0.4363636363636,0.444446021132103,0.452935779498683,
0.4545454545455,0.461363107469399,0.467498436348121,0.4727272727273,0.479753856203367,
0.486893986084007,0.4909090909091,0.497221599849583,0.50000000008049,0.506312509021862,
0.5090909090909,0.516218473166445,0.523276759559391,0.5272727272727,0.532501563651875,
0.539319216575929,0.5454545454545,0.553958903433111,0.562058004188518,0.5636363636364,
0.565000377410543,0.575117770912628,0.5818181818182,0.590215906719939,0.597499145923154,
0.6,0.607544534174367,0.615369925924941,0.6181818181818,0.624731105684524,
0.62999860391574,0.6363636363636,0.643337807374441,0.650372265605971,0.6545454545455,
0.66089219418957,0.662500695889797,0.668854008752732,0.6727272727273,0.680054448914732,
0.687247435925352,0.6909090909091,0.695001425050611,0.702251195725602,0.7090909090909,
0.7185504630727,0.7272727272727,0.72750003925074,0.737681027864929,0.7454545454545,
0.752946219661666,0.759998704383705,0.7636363636364,0.770877064964224,0.778316872209192,
0.7818181818182,0.788209682197035,0.792499059480986,0.798881081142189,0.8,
0.806989821147635,0.813987898664929,0.8181818181818,0.824642061622228,0.825001244508765,
0.831475911633545,0.8363636363636,0.844016413814636,0.85145248064292,0.8545454545455,
0.857501045096319,0.865473346951777,0.8727272727273,0.883510306083592,0.889999782950987,
0.8909090909091,0.899338083037124,0.908253221411253,0.9090909090909,0.916064223141442,
0.922498462510562,0.9272727272727,0.934348435683629,0.941558336299738,0.9454545454545,
0.951763846186177,0.954999762287945,0.961308833047529,0.9636363636364,0.970630376636409,
0.977577338426202,0.9818181818182,0.987501618298469,0.994118464170932,1.),
 .UNSPECIFIED.);
#210=B_SPLINE_CURVE_WITH_KNOTS('',3,(#14099,#14100,#14101,#14102,#14103,
#14104,#14105,#14106,#14107,#14108,#14109,#14110,#14111,#14112,#14113,#14114,
#14115,#14116,#14117,#14118,#14119,#14120,#14121,#14122,#14123,#14124,#14125,
#14126,#14127,#14128,#14129,#14130,#14131,#14132,#14133,#14134,#14135,#14136,
#14137,#14138,#14139,#14140,#14141),.UNSPECIFIED.,.F.,.F.,(4,3,3,3,3,3,
3,3,3,3,3,3,3,3,4),(0.,0.0875545420481924,0.172845777629218,0.25,0.335847439744804,
0.429706536572654,0.5,0.501528659337301,0.577112096262907,0.657242820363663,
0.735419949953638,0.75,0.839853036634623,0.941009610341032,1.),
 .UNSPECIFIED.);
#211=B_SPLINE_CURVE_WITH_KNOTS('',3,(#14142,#14143,#14144,#14145,#14146,
#14147,#14148,#14149,#14150,#14151,#14152,#14153,#14154,#14155,#14156,#14157,
#14158,#14159,#14160,#14161,#14162,#14163,#14164,#14165,#14166,#14167,#14168,
#14169,#14170,#14171,#14172,#14173,#14174,#14175,#14176,#14177,#14178,#14179,
#14180,#14181,#14182,#14183,#14184,#14185,#14186,#14187,#14188,#14189,#14190,
#14191,#14192,#14193,#14194,#14195,#14196,#14197,#14198,#14199,#14200,#14201,
#14202,#14203,#14204,#14205,#14206,#14207,#14208,#14209,#14210,#14211,#14212,
#14213,#14214,#14215,#14216,#14217,#14218,#14219,#14220,#14221,#14222,#14223,
#14224,#14225,#14226,#14227,#14228,#14229,#14230,#14231,#14232,#14233,#14234,
#14235,#14236,#14237,#14238,#14239,#14240,#14241,#14242,#14243,#14244,#14245,
#14246,#14247,#14248,#14249,#14250,#14251,#14252,#14253,#14254,#14255,#14256,
#14257,#14258,#14259,#14260,#14261,#14262,#14263,#14264,#14265,#14266,#14267,
#14268,#14269,#14270,#14271,#14272,#14273,#14274,#14275,#14276,#14277,#14278,
#14279,#14280,#14281,#14282,#14283,#14284,#14285,#14286,#14287,#14288,#14289,
#14290,#14291,#14292,#14293,#14294,#14295,#14296,#14297,#14298,#14299,#14300,
#14301,#14302,#14303,#14304,#14305,#14306,#14307,#14308,#14309,#14310,#14311,
#14312,#14313,#14314,#14315,#14316,#14317,#14318,#14319,#14320,#14321,#14322,
#14323,#14324,#14325,#14326,#14327,#14328,#14329,#14330,#14331,#14332,#14333,
#14334,#14335,#14336,#14337,#14338,#14339,#14340,#14341,#14342,#14343,#14344,
#14345,#14346,#14347,#14348,#14349,#14350,#14351,#14352,#14353,#14354,#14355,
#14356,#14357,#14358,#14359,#14360,#14361,#14362,#14363,#14364,#14365,#14366,
#14367,#14368,#14369,#14370,#14371,#14372,#14373,#14374,#14375,#14376,#14377,
#14378,#14379,#14380,#14381,#14382,#14383,#14384,#14385,#14386,#14387,#14388,
#14389,#14390,#14391,#14392,#14393,#14394,#14395,#14396,#14397,#14398,#14399,
#14400,#14401,#14402,#14403,#14404,#14405,#14406,#14407,#14408,#14409,#14410,
#14411,#14412,#14413,#14414,#14415,#14416,#14417,#14418,#14419,#14420,#14421,
#14422,#14423,#14424,#14425,#14426,#14427,#14428,#14429,#14430,#14431,#14432,
#14433,#14434,#14435,#14436,#14437,#14438,#14439,#14440,#14441,#14442,#14443,
#14444,#14445,#14446,#14447,#14448,#14449,#14450,#14451,#14452,#14453,#14454,
#14455,#14456,#14457,#14458,#14459,#14460,#14461,#14462,#14463,#14464,#14465,
#14466,#14467,#14468,#14469,#14470,#14471,#14472,#14473,#14474,#14475,#14476,
#14477,#14478,#14479,#14480,#14481,#14482,#14483,#14484,#14485,#14486,#14487,
#14488,#14489,#14490,#14491,#14492,#14493,#14494,#14495,#14496,#14497,#14498,
#14499,#14500,#14501,#14502,#14503,#14504,#14505,#14506,#14507,#14508,#14509,
#14510,#14511,#14512,#14513,#14514,#14515,#14516,#14517,#14518,#14519,#14520,
#14521,#14522,#14523,#14524,#14525,#14526,#14527,#14528,#14529,#14530,#14531,
#14532,#14533,#14534,#14535,#14536,#14537,#14538,#14539,#14540,#14541,#14542,
#14543,#14544,#14545,#14546,#14547,#14548,#14549,#14550,#14551,#14552,#14553,
#14554,#14555,#14556,#14557,#14558,#14559,#14560,#14561,#14562,#14563,#14564,
#14565,#14566,#14567,#14568,#14569,#14570,#14571,#14572,#14573,#14574,#14575,
#14576,#14577,#14578,#14579,#14580,#14581,#14582,#14583,#14584,#14585,#14586,
#14587,#14588,#14589,#14590,#14591,#14592,#14593,#14594,#14595,#14596,#14597,
#14598,#14599,#14600,#14601,#14602,#14603,#14604,#14605,#14606,#14607,#14608,
#14609,#14610,#14611,#14612,#14613,#14614,#14615,#14616,#14617,#14618,#14619,
#14620,#14621,#14622,#14623,#14624,#14625,#14626,#14627,#14628,#14629,#14630,
#14631,#14632,#14633,#14634,#14635,#14636,#14637,#14638,#14639,#14640,#14641,
#14642,#14643,#14644,#14645,#14646,#14647,#14648,#14649,#14650,#14651,#14652,
#14653,#14654,#14655,#14656,#14657,#14658,#14659,#14660,#14661,#14662,#14663,
#14664,#14665,#14666,#14667,#14668,#14669,#14670,#14671,#14672,#14673,#14674,
#14675,#14676,#14677,#14678,#14679,#14680,#14681,#14682,#14683,#14684,#14685,
#14686,#14687,#14688,#14689,#14690,#14691,#14692,#14693,#14694),
 .UNSPECIFIED.,.F.,.F.,(4,3,3,3,3,3,3,3,3,3,3,3,3,3,3,3,3,3,3,3,3,3,3,3,
3,3,3,3,3,3,3,3,3,3,3,3,3,3,3,3,3,3,3,3,3,3,3,3,3,3,3,3,3,3,3,3,3,3,3,3,
3,3,3,3,3,3,3,3,3,3,3,3,3,3,3,3,3,3,3,3,3,3,3,3,3,3,3,3,3,3,3,3,3,3,3,3,
3,3,3,3,3,3,3,3,3,3,3,3,3,3,3,3,3,3,3,3,3,3,3,3,3,3,3,3,3,3,3,3,3,3,3,3,
3,3,3,3,3,3,3,3,3,3,3,3,3,3,3,3,3,3,3,3,3,3,3,3,3,3,3,3,3,3,3,3,3,3,3,3,
3,3,3,3,3,3,3,3,3,3,3,3,3,3,3,3,4),(0.,0.00625925877606793,0.0124987776338276,
0.01694915254237,0.0234628389429566,0.0301365197563092,0.03389830508475,
0.039939545499986,0.0449988746104479,0.05084745762712,0.0573237266639023,
0.0638987543533824,0.06779661016949,0.0736716349306714,0.0774993881424457,
0.0833663385077112,0.08474576271186,0.0911673312994687,0.097628739000311,
0.1016949152542,0.107513390502593,0.110000096381758,0.115819871711832,0.1186440677966,
0.125101954653236,0.131545205429034,0.135593220339,0.141479707111713,0.142500758971051,
0.148398207639012,0.1525423728814,0.159137176793838,0.165656536878994,0.1694915254237,
0.175001153770122,0.181104985312047,0.1864406779661,0.193291692193679,0.199994170966203,
0.2033898305085,0.207501144893392,0.213996704784881,0.2203389830508,0.227648989561818,
0.2347073720192,0.2372881355932,0.240000783824308,0.247222805643388,0.2542372881356,
0.2627118644068,0.270472303966989,0.271186440678,0.272500297957408,0.28124476060672,
0.2881355932203,0.297798413322731,0.304999991245749,0.3050847457627,0.314508174872286,
0.3220338983051,0.330512021731217,0.337499649903534,0.3389830508475,0.346615949971126,
0.354646702577011,0.3559322033898,0.363033438864976,0.36999916343291,0.3728813559322,
0.379853325430446,0.387078943205471,0.3898305084746,0.396262716777213,0.402498837141285,
0.4067796610169,0.413421019420046,0.42023055686854,0.4237288135593,0.429797841794883,
0.434998879663639,0.4406779661017,0.447154148986795,0.453734297968399,0.4576271186441,
0.463508279082776,0.46749931747137,0.473370930095005,0.4745762711864,0.480995183542743,
0.487461530538509,0.4915254237288,0.497345526991346,0.500000003734252,0.505820187494761,
0.5084745762712,0.514924727844113,0.521366864166466,0.5254237288136,0.531295850594903,
0.532500689595533,0.538382527082556,0.5423728813559,0.548945254028873,0.555450031435156,
0.5593220338983,0.565001126342024,0.571071570720126,0.5762711864407,0.583082695457072,
0.589755631697393,0.5932203389831,0.597501167527672,0.60393592249075,0.6101694915254,
0.617407999264105,0.624410071112492,0.6271186440678,0.630000840110391,0.637106843597752,
0.6440677966102,0.65254237288135,0.66018060998796,0.6610169491525,0.662500353088121,
0.67098890654174,0.6779661016949,0.687400217120541,0.6949152542373,0.695000011705004,
0.704653651273056,0.7118644067797,0.720597517778143,0.727499705010129,0.728813559322,
0.736568079961608,0.744745446870372,0.7457627118644,0.752979538681499,0.759999219617496,
0.7627118644068,0.769740858446694,0.777036628436699,0.7796610169492,0.786153842811008,
0.79249885961846,0.7966101694915,0.803280942492585,0.810128713699996,0.8135593220339,
0.819661628475613,0.824998852078598,0.8305084745763,0.836998731347269,0.843600194647035,
0.8474576271186,0.853354320256033,0.857499247996783,0.863385148965559,0.864406779661,
0.870826069224946,0.877299244449807,0.8813559322034,0.887175557231284,0.88999991108234,
0.895818397253246,0.8983050847458,0.90474927177023,0.911193161122714,0.9152542372881,
0.921121621454917,0.922500619004355,0.928376243104466,0.9322033898305,0.938769848537038,
0.945274226985684,0.9491525423729,0.95500113157828,0.961043720040502,0.9661016949153,
0.972776378140131,0.97932286386849,0.9830508474576,0.987501227214035,0.993762571705703,
1.),.UNSPECIFIED.);
#212=B_SPLINE_CURVE_WITH_KNOTS('',3,(#15045,#15046,#15047,#15048,#15049,
#15050,#15051,#15052,#15053,#15054,#15055,#15056,#15057,#15058,#15059,#15060,
#15061,#15062,#15063,#15064,#15065,#15066,#15067,#15068,#15069,#15070,#15071,
#15072,#15073,#15074,#15075,#15076,#15077,#15078,#15079,#15080,#15081,#15082,
#15083,#15084,#15085,#15086,#15087,#15088,#15089,#15090,#15091,#15092,#15093,
#15094,#15095,#15096,#15097,#15098,#15099),.UNSPECIFIED.,.F.,.F.,(4,3,3,
3,3,3,3,3,3,3,3,3,3,3,3,3,3,3,4),(2.28557416296169E-7,4.45838597195228E-5,
0.103040149522257,0.1937218787354,0.25,0.251116964175455,0.330254232785831,
0.414362786403821,0.487704402379652,0.49847134002181,0.5,0.590018211501603,
0.650623800434858,0.733876213552138,0.75,0.804169141593649,0.887250644428625,
0.959806362374165,1.),.UNSPECIFIED.);
#213=B_SPLINE_CURVE_WITH_KNOTS('',3,(#15346,#15347,#15348,#15349,#15350,
#15351,#15352,#15353,#15354,#15355,#15356,#15357,#15358,#15359,#15360,#15361,
#15362,#15363,#15364,#15365,#15366,#15367,#15368,#15369,#15370,#15371,#15372,
#15373,#15374,#15375,#15376,#15377,#15378,#15379,#15380,#15381,#15382,#15383,
#15384,#15385,#15386,#15387,#15388,#15389,#15390,#15391,#15392,#15393,#15394,
#15395,#15396,#15397,#15398,#15399,#15400,#15401,#15402,#15403,#15404,#15405,
#15406,#15407,#15408,#15409,#15410,#15411,#15412,#15413,#15414,#15415,#15416,
#15417,#15418,#15419,#15420,#15421,#15422,#15423,#15424,#15425,#15426,#15427,
#15428,#15429,#15430,#15431,#15432,#15433,#15434,#15435,#15436,#15437,#15438,
#15439,#15440,#15441,#15442,#15443,#15444,#15445,#15446,#15447,#15448,#15449,
#15450,#15451,#15452,#15453,#15454,#15455,#15456,#15457,#15458,#15459,#15460,
#15461,#15462,#15463,#15464,#15465,#15466,#15467,#15468,#15469,#15470,#15471,
#15472,#15473,#15474,#15475,#15476,#15477,#15478,#15479,#15480,#15481,#15482,
#15483,#15484,#15485,#15486,#15487,#15488,#15489,#15490,#15491,#15492,#15493,
#15494,#15495,#15496,#15497,#15498,#15499,#15500,#15501,#15502,#15503,#15504,
#15505,#15506,#15507,#15508,#15509,#15510,#15511,#15512,#15513,#15514,#15515,
#15516,#15517,#15518,#15519,#15520,#15521,#15522,#15523,#15524,#15525,#15526,
#15527,#15528,#15529,#15530,#15531,#15532,#15533,#15534,#15535,#15536,#15537,
#15538,#15539,#15540,#15541,#15542,#15543,#15544,#15545,#15546,#15547,#15548,
#15549,#15550,#15551,#15552,#15553,#15554,#15555,#15556,#15557,#15558,#15559,
#15560,#15561,#15562,#15563,#15564,#15565,#15566,#15567,#15568,#15569,#15570,
#15571,#15572,#15573,#15574,#15575,#15576,#15577,#15578,#15579,#15580,#15581,
#15582,#15583,#15584,#15585,#15586,#15587,#15588,#15589,#15590,#15591,#15592,
#15593,#15594,#15595,#15596,#15597,#15598,#15599,#15600,#15601,#15602,#15603,
#15604,#15605,#15606,#15607,#15608,#15609,#15610,#15611,#15612,#15613,#15614,
#15615,#15616,#15617,#15618,#15619,#15620,#15621,#15622,#15623,#15624,#15625,
#15626,#15627,#15628,#15629,#15630,#15631,#15632,#15633,#15634,#15635,#15636,
#15637,#15638,#15639,#15640,#15641,#15642,#15643,#15644,#15645,#15646,#15647,
#15648,#15649,#15650,#15651,#15652,#15653,#15654,#15655,#15656,#15657,#15658,
#15659,#15660,#15661,#15662,#15663,#15664,#15665,#15666,#15667,#15668,#15669,
#15670,#15671,#15672,#15673,#15674,#15675,#15676,#15677,#15678,#15679,#15680,
#15681,#15682,#15683,#15684,#15685,#15686,#15687,#15688,#15689,#15690,#15691,
#15692,#15693,#15694,#15695,#15696,#15697,#15698,#15699,#15700,#15701,#15702,
#15703,#15704,#15705,#15706,#15707,#15708,#15709,#15710,#15711,#15712,#15713,
#15714,#15715,#15716,#15717,#15718,#15719,#15720,#15721,#15722,#15723,#15724,
#15725,#15726,#15727,#15728,#15729,#15730,#15731,#15732,#15733,#15734,#15735,
#15736,#15737,#15738,#15739,#15740,#15741,#15742,#15743,#15744,#15745,#15746,
#15747,#15748,#15749,#15750,#15751,#15752,#15753,#15754,#15755,#15756,#15757,
#15758,#15759,#15760,#15761,#15762,#15763,#15764,#15765,#15766,#15767,#15768,
#15769,#15770,#15771,#15772,#15773,#15774,#15775,#15776,#15777,#15778,#15779,
#15780,#15781,#15782,#15783,#15784,#15785,#15786,#15787,#15788,#15789,#15790,
#15791,#15792,#15793,#15794,#15795,#15796,#15797,#15798,#15799,#15800,#15801,
#15802,#15803,#15804,#15805,#15806,#15807,#15808,#15809,#15810,#15811,#15812,
#15813,#15814,#15815,#15816,#15817,#15818,#15819,#15820,#15821,#15822,#15823,
#15824,#15825,#15826,#15827,#15828,#15829,#15830,#15831,#15832,#15833,#15834,
#15835,#15836,#15837,#15838,#15839,#15840,#15841,#15842,#15843,#15844,#15845,
#15846,#15847,#15848,#15849,#15850,#15851,#15852,#15853,#15854,#15855,#15856,
#15857,#15858,#15859,#15860,#15861,#15862,#15863,#15864,#15865,#15866,#15867,
#15868,#15869,#15870,#15871,#15872,#15873,#15874,#15875,#15876,#15877,#15878,
#15879,#15880,#15881,#15882,#15883,#15884,#15885,#15886,#15887,#15888,#15889,
#15890,#15891,#15892,#15893,#15894,#15895,#15896,#15897,#15898),
 .UNSPECIFIED.,.F.,.F.,(4,3,3,3,3,3,3,3,3,3,3,3,3,3,3,3,3,3,3,3,3,3,3,3,
3,3,3,3,3,3,3,3,3,3,3,3,3,3,3,3,3,3,3,3,3,3,3,3,3,3,3,3,3,3,3,3,3,3,3,3,
3,3,3,3,3,3,3,3,3,3,3,3,3,3,3,3,3,3,3,3,3,3,3,3,3,3,3,3,3,3,3,3,3,3,3,3,
3,3,3,3,3,3,3,3,3,3,3,3,3,3,3,3,3,3,3,3,3,3,3,3,3,3,3,3,3,3,3,3,3,3,3,3,
3,3,3,3,3,3,3,3,3,3,3,3,3,3,3,3,3,3,3,3,3,3,3,3,3,3,3,3,3,3,3,3,3,3,3,3,
3,3,3,3,3,3,3,3,3,3,3,3,3,3,3,3,4),(0.,0.00625707247057022,0.0124987693041953,
0.01694915254237,0.0234597676321377,0.030130415664672,0.03389830508475,
0.0399367007525247,0.0449988678636083,0.05084745762712,0.0573205787421996,
0.0638925612737411,0.06779661016949,0.0736684880648363,0.0774993821578474,
0.0833631085591902,0.08474576271186,0.0911641141481979,0.097622449623175,
0.1016949152542,0.107509985014228,0.11000009299126,0.115816381204191,0.1186440677966,
0.125098471554685,0.131538419892334,0.135593220339,0.141475976279384,0.142500758333531,
0.148394384381762,0.1525423728814,0.159133140168786,0.165648703850875,0.1694915254237,
0.175001155269066,0.181100725849585,0.1864406779661,0.193286624103164,0.199984396474713,
0.2033898305085,0.207501147182458,0.213991841709094,0.2203389830508,0.227641776056833,
0.234693622399377,0.2372881355932,0.240000785292989,0.247217140945622,0.2542372881356,
0.2627118644068,0.27046083374304,0.271186440678,0.272500297585015,0.281238797730683,
0.2881355932203,0.297779235715604,0.304999989764099,0.3050847457627,0.314497758523359,
0.3220338983051,0.330516391338742,0.337499647052717,0.3389830508475,0.346610725412041,
0.354635740839695,0.3559322033898,0.363032643660964,0.369999158245744,0.3728813559322,
0.379849543493191,0.387071287109133,0.3898305084746,0.39626048216284,0.402498830192386,
0.4067796610169,0.41341773856689,0.420224034400144,0.4237288135593,0.429795057904492,
0.434998872355421,0.4406779661017,0.447151018279596,0.453728136179621,0.4576271186441,
0.463505178577456,0.467499311365647,0.473367745831533,0.4745762711864,0.480991993708343,
0.48745528955393,0.4915254237288,0.49734215213837,0.500000000044217,0.50581672845434,
0.5084745762712,0.514921286064733,0.521360156754795,0.5254237288136,0.531292163279376,
0.532500688634353,0.538378748567485,0.5423728813559,0.548941304568806,0.555442363344076,
0.5593220338983,0.565001127644577,0.571067371989645,0.5762711864407,0.583077792237934,
0.58974616604175,0.5932203389831,0.597501169807617,0.603931143495856,0.6101694915254,
0.617401150396015,0.624396992337254,0.6271186440678,0.630000841754257,0.637101282025258,
0.6440677966102,0.652108496201867,0.659748125429028,0.6610169491525,0.662500352947285,
0.670982845980953,0.6779661016949,0.687379114455814,0.6949152542373,0.695000010235901,
0.704643652731264,0.7118644067797,0.720602906926292,0.727499702414991,0.728813559322,
0.736562528658307,0.744733729676818,0.7457627118644,0.752979067516863,0.75999921470701,
0.7627118644068,0.769736974051562,0.777028740384925,0.7796610169492,0.786151711475952,
0.792498852817539,0.7966101694915,0.803277624820126,0.810122107164893,0.8135593220339,
0.819658892614575,0.824998844730939,0.8305084745763,0.836995593846511,0.843594013502594,
0.8474576271186,0.853351253166922,0.857499241666464,0.863381997606931,0.864406779661,
0.870822899633561,0.8772930400371,0.8813559322034,0.887172220416142,0.889999907008734,
0.895814976768646,0.8983050847458,0.904745868788263,0.911186525219332,0.9152542372881,
0.92111796368911,0.922500617842136,0.928372495737183,0.9322033898305,0.93876593182826,
0.945266618311092,0.9491525423729,0.955001132136413,0.961039527803894,0.9661016949153,
0.972771935762613,0.979314297120634,0.9830508474576,0.987501230695801,0.993758303164287,
1.),.UNSPECIFIED.);
#214=B_SPLINE_CURVE_WITH_KNOTS('',3,(#15900,#15901,#15902,#15903,#15904,
#15905,#15906,#15907,#15908,#15909,#15910,#15911,#15912,#15913,#15914,#15915,
#15916,#15917,#15918,#15919,#15920,#15921),.UNSPECIFIED.,.F.,.F.,(4,2,2,
2,2,2,2,2,2,2,4),(-0.108366379525748,-0.101004560326757,-0.0935005570164099,
-0.0775237436752796,-0.0642908492457915,-0.0539096504263199,-0.0435454398611879,
-0.0302727818609328,-0.0143408019654358,-0.00710487439831416,-1.34996523534921E-6),
 .UNSPECIFIED.);
#215=B_SPLINE_CURVE_WITH_KNOTS('',3,(#15922,#15923,#15924,#15925,#15926,
#15927,#15928,#15929,#15930,#15931,#15932,#15933,#15934,#15935,#15936,#15937,
#15938,#15939,#15940,#15941,#15942,#15943,#15944,#15945,#15946,#15947,#15948,
#15949,#15950,#15951,#15952,#15953,#15954,#15955,#15956,#15957,#15958,#15959,
#15960,#15961,#15962,#15963,#15964,#15965,#15966,#15967,#15968,#15969,#15970,
#15971,#15972,#15973,#15974,#15975,#15976,#15977,#15978,#15979,#15980,#15981,
#15982,#15983,#15984,#15985,#15986,#15987,#15988,#15989,#15990,#15991,#15992,
#15993,#15994,#15995,#15996,#15997,#15998,#15999,#16000,#16001,#16002,#16003,
#16004,#16005,#16006,#16007,#16008,#16009,#16010,#16011,#16012,#16013,#16014,
#16015,#16016,#16017,#16018,#16019,#16020,#16021,#16022,#16023,#16024,#16025,
#16026,#16027,#16028,#16029,#16030,#16031,#16032,#16033,#16034,#16035,#16036,
#16037,#16038,#16039,#16040,#16041,#16042,#16043,#16044,#16045,#16046,#16047,
#16048,#16049,#16050,#16051,#16052,#16053,#16054,#16055,#16056,#16057,#16058,
#16059,#16060,#16061,#16062,#16063,#16064,#16065,#16066,#16067,#16068,#16069,
#16070,#16071,#16072,#16073,#16074,#16075,#16076,#16077,#16078,#16079,#16080,
#16081,#16082,#16083,#16084,#16085,#16086,#16087,#16088,#16089,#16090,#16091,
#16092,#16093,#16094,#16095,#16096,#16097,#16098,#16099,#16100,#16101,#16102,
#16103,#16104,#16105,#16106,#16107,#16108,#16109,#16110,#16111,#16112,#16113,
#16114,#16115,#16116,#16117,#16118,#16119,#16120,#16121,#16122,#16123,#16124,
#16125,#16126,#16127,#16128,#16129,#16130,#16131,#16132,#16133,#16134,#16135,
#16136,#16137,#16138,#16139,#16140,#16141,#16142,#16143,#16144,#16145,#16146,
#16147,#16148,#16149,#16150,#16151,#16152,#16153,#16154,#16155,#16156,#16157,
#16158,#16159,#16160,#16161,#16162,#16163,#16164,#16165,#16166,#16167,#16168,
#16169,#16170,#16171,#16172,#16173,#16174,#16175,#16176,#16177,#16178,#16179,
#16180,#16181,#16182,#16183,#16184,#16185,#16186,#16187,#16188,#16189,#16190,
#16191,#16192,#16193,#16194,#16195,#16196,#16197,#16198,#16199,#16200,#16201,
#16202,#16203,#16204,#16205,#16206,#16207,#16208,#16209,#16210,#16211,#16212,
#16213,#16214,#16215,#16216,#16217,#16218,#16219,#16220,#16221,#16222,#16223,
#16224,#16225,#16226,#16227,#16228,#16229,#16230,#16231,#16232,#16233,#16234,
#16235,#16236,#16237,#16238,#16239,#16240,#16241,#16242,#16243,#16244,#16245,
#16246,#16247,#16248,#16249,#16250,#16251,#16252,#16253,#16254,#16255,#16256,
#16257,#16258,#16259,#16260,#16261,#16262,#16263,#16264,#16265,#16266,#16267,
#16268,#16269,#16270,#16271,#16272,#16273,#16274,#16275,#16276,#16277,#16278,
#16279,#16280,#16281,#16282,#16283,#16284,#16285,#16286,#16287,#16288,#16289,
#16290,#16291,#16292,#16293,#16294,#16295,#16296,#16297,#16298,#16299,#16300,
#16301,#16302,#16303,#16304,#16305,#16306,#16307,#16308,#16309,#16310,#16311,
#16312,#16313,#16314,#16315,#16316,#16317,#16318,#16319,#16320,#16321,#16322,
#16323,#16324,#16325,#16326,#16327,#16328,#16329,#16330,#16331,#16332,#16333,
#16334,#16335,#16336,#16337,#16338,#16339,#16340,#16341,#16342,#16343,#16344,
#16345,#16346,#16347,#16348,#16349,#16350,#16351,#16352,#16353,#16354,#16355,
#16356,#16357,#16358,#16359,#16360,#16361,#16362,#16363,#16364,#16365,#16366,
#16367,#16368,#16369,#16370,#16371,#16372,#16373,#16374,#16375,#16376,#16377,
#16378,#16379,#16380,#16381,#16382,#16383,#16384,#16385,#16386,#16387,#16388,
#16389,#16390,#16391,#16392,#16393,#16394,#16395,#16396,#16397,#16398,#16399,
#16400,#16401,#16402,#16403,#16404,#16405,#16406,#16407,#16408,#16409,#16410,
#16411,#16412,#16413,#16414,#16415,#16416,#16417,#16418,#16419,#16420,#16421,
#16422,#16423,#16424,#16425,#16426,#16427,#16428,#16429,#16430,#16431,#16432,
#16433,#16434,#16435,#16436,#16437,#16438),.UNSPECIFIED.,.F.,.F.,(4,3,3,
3,3,3,3,3,3,3,3,3,3,3,3,3,3,3,3,3,3,3,3,3,3,3,3,3,3,3,3,3,3,3,3,3,3,3,3,
3,3,3,3,3,3,3,3,3,3,3,3,3,3,3,3,3,3,3,3,3,3,3,3,3,3,3,3,3,3,3,3,3,3,3,3,
3,3,3,3,3,3,3,3,3,3,3,3,3,3,3,3,3,3,3,3,3,3,3,3,3,3,3,3,3,3,3,3,3,3,3,3,
3,3,3,3,3,3,3,3,3,3,3,3,3,3,3,3,3,3,3,3,3,3,3,3,3,3,3,3,3,3,3,3,3,3,3,3,
3,3,3,3,3,3,3,3,3,3,3,3,3,3,3,3,3,3,3,3,3,3,3,3,3,4),(0.,0.00661684587379473,
0.0124983817015441,0.01818181818182,0.0250973637786607,0.0321069452297743,
0.03636363636364,0.0426727071234223,0.045000237712052,0.0513095384438299,
0.05454545454545,0.0617456257730734,0.0688539134549294,0.07272727272727,
0.0775015374894184,0.0844748515404932,0.09090909090909,0.099999999999995,
0.108428992129646,0.1090909090909,0.110000217049001,0.120783250406619,0.1272727272727,
0.135245029127397,0.142498954903679,0.1454545454545,0.15285832598237,0.160506900312804,
0.1636363636364,0.170111030761004,0.174998755491224,0.181458998931522,0.1818181818182,
0.188790646918454,0.195802632396944,0.2,0.206382021661163,0.207500940519022,
0.213892440897663,0.2181818181818,0.225620516663835,0.232894893756836,0.2363636363636,
0.240001295616291,0.247492969823552,0.2545454545455,0.264726443160272,0.27249996074925,
0.2727272727273,0.282186826708758,0.2909090909091,0.298158861584068,0.304998574949384,
0.3090909090909,0.316250191676584,0.32358191434256,0.3272727272727,0.333626040135738,
0.337499304110204,0.343846043754328,0.3454545454545,0.352469372214463,0.35947119982488,
0.3636363636364,0.370001396084259,0.376550683587071,0.3818181818182,0.389651329370141,
0.397226012190253,0.4,0.402500854076842,0.410898578978884,0.4181818181818,
0.428299211683941,0.434999622589457,0.4363636363636,0.444446021132232,0.452935779498618,
0.4545454545455,0.461363107469256,0.467498436348121,0.4727272727273,0.479753856203258,
0.48689398608381,0.4909090909091,0.497221599850067,0.499999999973427,0.506312508914082,
0.5090909090909,0.516218473166076,0.523276759558518,0.5272727272727,0.532501563651881,
0.539319216575566,0.5454545454545,0.553958903432471,0.562058004187475,0.5636363636364,
0.565000377410548,0.575117770912058,0.5818181818182,0.590215906720766,0.597499145923165,
0.6,0.607544534174676,0.615369925925628,0.6181818181818,0.624731105684416,
0.629998603915741,0.6363636363636,0.643337807374075,0.650372265605402,0.6545454545455,
0.66089219418975,0.662500695889806,0.668854008752749,0.6727272727273,0.68005444891509,
0.687247435926077,0.6909090909091,0.695001425050612,0.702251195725806,0.7090909090909,
0.718550463073272,0.7272727272727,0.727500039250745,0.737681027863759,0.7454545454545,
0.752946219661041,0.759998704383708,0.7636363636364,0.770877064963762,0.778316872208324,
0.7818181818182,0.788209682196738,0.792499059480988,0.798881081142194,0.8,
0.806989821147026,0.81398789866388,0.8181818181818,0.824642061622016,0.825001244508772,
0.831475911633192,0.8363636363636,0.844016413814312,0.851452480642349,0.8545454545455,
0.857501045096315,0.865473346951193,0.8727272727273,0.883510306083999,0.889999782950997,
0.8909090909091,0.899338083038148,0.908253221413727,0.9090909090909,0.916064223141629,
0.922498462510559,0.9272727272727,0.934348435683951,0.941558336300596,0.9454545454545,
0.951763846186328,0.954999762287933,0.961308833047855,0.9636363636364,0.970630376636484,
0.977577338426374,0.9818181818182,0.987501618298468,0.994118464171033,1.),
 .UNSPECIFIED.);
#216=B_SPLINE_CURVE_WITH_KNOTS('',3,(#16684,#16685,#16686,#16687,#16688,
#16689,#16690,#16691,#16692,#16693,#16694,#16695,#16696,#16697,#16698,#16699,
#16700,#16701,#16702,#16703,#16704,#16705),.UNSPECIFIED.,.F.,.F.,(4,2,2,
2,2,2,2,2,2,2,4),(-0.107848148767986,-0.10078133624504,-0.0935834381175982,
-0.0777250902731328,-0.0645137902634984,-0.0541974885556667,-0.0438642827821331,
-0.0306925477519394,-0.0147895883407361,-0.00732502687635996,-1.25961705293921E-6),
 .UNSPECIFIED.);
#217=B_SPLINE_CURVE_WITH_KNOTS('',3,(#16826,#16827,#16828,#16829),
 .UNSPECIFIED.,.F.,.F.,(4,4),(-0.288701302460675,0.),.UNSPECIFIED.);
#218=B_SPLINE_CURVE_WITH_KNOTS('',3,(#16830,#16831,#16832,#16833),
 .UNSPECIFIED.,.F.,.F.,(4,4),(-0.939904999188834,-0.651203696728158),
 .UNSPECIFIED.);
#219=B_SPLINE_CURVE_WITH_KNOTS('',3,(#16836,#16837,#16838,#16839),
 .UNSPECIFIED.,.F.,.F.,(4,4),(0.651203696728158,0.939904999188834),
 .UNSPECIFIED.);
#220=B_SPLINE_CURVE_WITH_KNOTS('',3,(#16849,#16850,#16851,#16852),
 .UNSPECIFIED.,.F.,.F.,(4,4),(0.,0.288701302460675),.UNSPECIFIED.);
#221=OPEN_SHELL('',(#5698,#5699));
#222=OPEN_SHELL('',(#5700,#5701));
#223=OPEN_SHELL('',(#5804,#5805));
#224=OPEN_SHELL('',(#5806,#5807));
#225=OPEN_SHELL('',(#5821,#5822));
#226=OPEN_SHELL('',(#5823,#5824));
#227=OPEN_SHELL('',(#5864,#5865));
#228=OPEN_SHELL('',(#5877,#5878));
#229=OPEN_SHELL('',(#5914,#5915));
#230=OPEN_SHELL('',(#5916,#5917));
#231=OPEN_SHELL('',(#5918,#5919));
#232=OPEN_SHELL('',(#5920,#5921));
#233=OPEN_SHELL('',(#5922,#5923));
#234=OPEN_SHELL('',(#5954,#5955));
#235=OPEN_SHELL('',(#5974,#5975));
#236=OPEN_SHELL('',(#5981,#5982));
#237=OPEN_SHELL('',(#5983,#5984));
#238=OPEN_SHELL('',(#5993,#5994));
#239=SHELL_BASED_SURFACE_MODEL('Body2',(#221));
#240=SHELL_BASED_SURFACE_MODEL('Body3',(#222));
#241=SHELL_BASED_SURFACE_MODEL('Body2',(#223));
#242=SHELL_BASED_SURFACE_MODEL('Body3',(#224));
#243=SHELL_BASED_SURFACE_MODEL('Body2',(#225));
#244=SHELL_BASED_SURFACE_MODEL('Body3',(#226));
#245=SHELL_BASED_SURFACE_MODEL('Body2',(#227));
#246=SHELL_BASED_SURFACE_MODEL('Body2',(#228));
#247=SHELL_BASED_SURFACE_MODEL('Body2',(#229));
#248=SHELL_BASED_SURFACE_MODEL('Body3',(#230));
#249=SHELL_BASED_SURFACE_MODEL('Body4',(#231));
#250=SHELL_BASED_SURFACE_MODEL('Body5',(#232));
#251=SHELL_BASED_SURFACE_MODEL('Body6',(#233));
#252=SHELL_BASED_SURFACE_MODEL('Body2',(#234));
#253=SHELL_BASED_SURFACE_MODEL('Body2',(#235));
#254=SHELL_BASED_SURFACE_MODEL('Body2',(#236));
#255=SHELL_BASED_SURFACE_MODEL('Body3',(#237));
#256=SHELL_BASED_SURFACE_MODEL('Body2',(#238));
#257=CONICAL_SURFACE('',#6271,8.999999999749,0.785398163397448);
#258=CONICAL_SURFACE('',#6274,8.999999999749,0.785398163397448);
#259=CONICAL_SURFACE('',#6277,8.999999999749,0.785398163397448);
#260=CONICAL_SURFACE('',#6280,8.999999999749,0.785398163397448);
#261=CONICAL_SURFACE('',#6390,1.375,0.785398163397448);
#262=CONICAL_SURFACE('',#6393,5.187242561534,0.0698131700797732);
#263=CONICAL_SURFACE('',#6396,5.187242561534,0.0698131700797732);
#264=SHAPE_REPRESENTATION_RELATIONSHIP('SRR','None',#17185,#280);
#265=SHAPE_REPRESENTATION_RELATIONSHIP('SRR','None',#17187,#281);
#266=SHAPE_REPRESENTATION_RELATIONSHIP('SRR','None',#17188,#282);
#267=SHAPE_REPRESENTATION_RELATIONSHIP('SRR','None',#17189,#283);
#268=SHAPE_REPRESENTATION_RELATIONSHIP('SRR','None',#17191,#284);
#269=SHAPE_REPRESENTATION_RELATIONSHIP('SRR','None',#17193,#285);
#270=SHAPE_REPRESENTATION_RELATIONSHIP('SRR','None',#17194,#286);
#271=SHAPE_REPRESENTATION_RELATIONSHIP('SRR','None',#17195,#287);
#272=SHAPE_REPRESENTATION_RELATIONSHIP('SRR','None',#17197,#288);
#273=SHAPE_REPRESENTATION_RELATIONSHIP('SRR','None',#17198,#289);
#274=SHAPE_REPRESENTATION_RELATIONSHIP('SRR','None',#17199,#290);
#275=SHAPE_REPRESENTATION_RELATIONSHIP('SRR','None',#17200,#291);
#276=SHAPE_REPRESENTATION_RELATIONSHIP('SRR','None',#17202,#292);
#277=SHAPE_REPRESENTATION_RELATIONSHIP('SRR','None',#17203,#293);
#278=SHAPE_REPRESENTATION_RELATIONSHIP('SRR','None',#17204,#294);
#279=SHAPE_REPRESENTATION_RELATIONSHIP('SRR','None',#17205,#295);
#280=ADVANCED_BREP_SHAPE_REPRESENTATION('',(#330),#17092);
#281=ADVANCED_BREP_SHAPE_REPRESENTATION('',(#331),#17094);
#282=ADVANCED_BREP_SHAPE_REPRESENTATION('',(#332),#17095);
#283=ADVANCED_BREP_SHAPE_REPRESENTATION('',(#333),#17096);
#284=ADVANCED_BREP_SHAPE_REPRESENTATION('',(#334),#17098);
#285=ADVANCED_BREP_SHAPE_REPRESENTATION('',(#335),#17100);
#286=ADVANCED_BREP_SHAPE_REPRESENTATION('',(#336),#17101);
#287=ADVANCED_BREP_SHAPE_REPRESENTATION('',(#337),#17102);
#288=ADVANCED_BREP_SHAPE_REPRESENTATION('',(#338),#17104);
#289=ADVANCED_BREP_SHAPE_REPRESENTATION('',(#339),#17105);
#290=ADVANCED_BREP_SHAPE_REPRESENTATION('',(#340),#17106);
#291=ADVANCED_BREP_SHAPE_REPRESENTATION('',(#341),#17107);
#292=ADVANCED_BREP_SHAPE_REPRESENTATION('',(#342),#17109);
#293=ADVANCED_BREP_SHAPE_REPRESENTATION('',(#343),#17110);
#294=ADVANCED_BREP_SHAPE_REPRESENTATION('',(#344),#17111);
#295=ADVANCED_BREP_SHAPE_REPRESENTATION('',(#345),#17112);
#296=STYLED_ITEM('',(#17298),#330);
#297=STYLED_ITEM('',(#17298),#331);
#298=STYLED_ITEM('',(#17298),#239);
#299=STYLED_ITEM('',(#17298),#240);
#300=STYLED_ITEM('',(#17298),#332);
#301=STYLED_ITEM('',(#17298),#241);
#302=STYLED_ITEM('',(#17298),#242);
#303=STYLED_ITEM('',(#17298),#333);
#304=STYLED_ITEM('',(#17298),#243);
#305=STYLED_ITEM('',(#17298),#244);
#306=STYLED_ITEM('',(#17298),#334);
#307=STYLED_ITEM('',(#17298),#335);
#308=STYLED_ITEM('',(#17298),#245);
#309=STYLED_ITEM('',(#17298),#336);
#310=STYLED_ITEM('',(#17298),#246);
#311=STYLED_ITEM('',(#17298),#337);
#312=STYLED_ITEM('',(#17298),#338);
#313=STYLED_ITEM('',(#17298),#247);
#314=STYLED_ITEM('',(#17298),#248);
#315=STYLED_ITEM('',(#17298),#249);
#316=STYLED_ITEM('',(#17298),#250);
#317=STYLED_ITEM('',(#17298),#251);
#318=STYLED_ITEM('',(#17298),#339);
#319=STYLED_ITEM('',(#17298),#340);
#320=STYLED_ITEM('',(#17298),#341);
#321=STYLED_ITEM('',(#17298),#252);
#322=STYLED_ITEM('',(#17298),#342);
#323=STYLED_ITEM('',(#17298),#253);
#324=STYLED_ITEM('',(#17298),#343);
#325=STYLED_ITEM('',(#17298),#254);
#326=STYLED_ITEM('',(#17298),#255);
#327=STYLED_ITEM('',(#17298),#344);
#328=STYLED_ITEM('',(#17298),#256);
#329=STYLED_ITEM('',(#17298),#345);
#330=MANIFOLD_SOLID_BREP('Body1',#6016);
#331=MANIFOLD_SOLID_BREP('Body1',#6017);
#332=MANIFOLD_SOLID_BREP('Body1',#6018);
#333=MANIFOLD_SOLID_BREP('Body1',#6019);
#334=MANIFOLD_SOLID_BREP('Body1',#6020);
#335=MANIFOLD_SOLID_BREP('Body1',#6021);
#336=MANIFOLD_SOLID_BREP('Body1',#6022);
#337=MANIFOLD_SOLID_BREP('Body1',#6023);
#338=MANIFOLD_SOLID_BREP('Body1',#6024);
#339=MANIFOLD_SOLID_BREP('Body1',#6025);
#340=MANIFOLD_SOLID_BREP('Body1',#6026);
#341=MANIFOLD_SOLID_BREP('Body1',#6027);
#342=MANIFOLD_SOLID_BREP('Body1',#6028);
#343=MANIFOLD_SOLID_BREP('Body1',#6029);
#344=MANIFOLD_SOLID_BREP('Body1',#6030);
#345=MANIFOLD_SOLID_BREP('Body1',#6031);
#346=CYLINDRICAL_SURFACE('',#6231,2.5);
#347=CYLINDRICAL_SURFACE('',#6232,2.5);
#348=CYLINDRICAL_SURFACE('',#6233,2.5);
#349=CYLINDRICAL_SURFACE('',#6234,2.5);
#350=CYLINDRICAL_SURFACE('',#6235,1.5);
#351=CYLINDRICAL_SURFACE('',#6240,1.5);
#352=CYLINDRICAL_SURFACE('',#6254,2.5);
#353=CYLINDRICAL_SURFACE('',#6266,2.5);
#354=CYLINDRICAL_SURFACE('',#6267,2.5);
#355=CYLINDRICAL_SURFACE('',#6268,2.5);
#356=CYLINDRICAL_SURFACE('',#6269,1.75);
#357=CYLINDRICAL_SURFACE('',#6270,1.75);
#358=CYLINDRICAL_SURFACE('',#6284,10.);
#359=CYLINDRICAL_SURFACE('',#6286,10.);
#360=CYLINDRICAL_SURFACE('',#6288,10.);
#361=CYLINDRICAL_SURFACE('',#6290,10.);
#362=CYLINDRICAL_SURFACE('',#6291,2.);
#363=CYLINDRICAL_SURFACE('',#6296,2.);
#364=CYLINDRICAL_SURFACE('',#6304,4.5);
#365=CYLINDRICAL_SURFACE('',#6312,2.5);
#366=CYLINDRICAL_SURFACE('',#6320,4.5);
#367=CYLINDRICAL_SURFACE('',#6323,1.);
#368=CYLINDRICAL_SURFACE('',#6327,1.);
#369=CYLINDRICAL_SURFACE('',#6333,1.);
#370=CYLINDRICAL_SURFACE('',#6336,1.);
#371=CYLINDRICAL_SURFACE('',#6349,1.);
#372=CYLINDRICAL_SURFACE('',#6352,1.);
#373=CYLINDRICAL_SURFACE('',#6357,1.);
#374=CYLINDRICAL_SURFACE('',#6361,1.);
#375=CYLINDRICAL_SURFACE('',#6364,1.);
#376=CYLINDRICAL_SURFACE('',#6369,1.);
#377=CYLINDRICAL_SURFACE('',#6374,1.);
#378=CYLINDRICAL_SURFACE('',#6375,1.);
#379=CYLINDRICAL_SURFACE('',#6379,1.);
#380=CYLINDRICAL_SURFACE('',#6385,1.);
#381=CYLINDRICAL_SURFACE('',#6386,4.);
#382=CYLINDRICAL_SURFACE('',#6392,1.25);
#383=CYLINDRICAL_SURFACE('',#6414,2.625);
#384=CYLINDRICAL_SURFACE('',#6417,1.75);
#385=CYLINDRICAL_SURFACE('',#6425,1.75);
#386=CYLINDRICAL_SURFACE('',#6426,2.625);
#387=CYLINDRICAL_SURFACE('',#6432,1.);
#388=CYLINDRICAL_SURFACE('',#6442,2.);
#389=CYLINDRICAL_SURFACE('',#6443,1.);
#390=CYLINDRICAL_SURFACE('',#6446,1.);
#391=CYLINDRICAL_SURFACE('',#6451,1.);
#392=CYLINDRICAL_SURFACE('',#6452,1.);
#393=CYLINDRICAL_SURFACE('',#6456,1.);
#394=CYLINDRICAL_SURFACE('',#6458,1.);
#395=CYLINDRICAL_SURFACE('',#6462,1.);
#396=CYLINDRICAL_SURFACE('',#6467,2.);
#397=CYLINDRICAL_SURFACE('',#6475,2.);
#398=CYLINDRICAL_SURFACE('',#6478,1.);
#399=CYLINDRICAL_SURFACE('',#6483,1.);
#400=CYLINDRICAL_SURFACE('',#6485,1.);
#401=CYLINDRICAL_SURFACE('',#6490,1.);
#402=CYLINDRICAL_SURFACE('',#6493,1.);
#403=CYLINDRICAL_SURFACE('',#6494,1.);
#404=CYLINDRICAL_SURFACE('',#6497,1.);
#405=CYLINDRICAL_SURFACE('',#6502,1.);
#406=CYLINDRICAL_SURFACE('',#6503,1.);
#407=CYLINDRICAL_SURFACE('',#6507,1.);
#408=CYLINDRICAL_SURFACE('',#6513,3.);
#409=CYLINDRICAL_SURFACE('',#6518,3.);
#410=CYLINDRICAL_SURFACE('',#6534,2.75);
#411=CYLINDRICAL_SURFACE('',#6536,2.75);
#412=CYLINDRICAL_SURFACE('',#6540,1.75);
#413=CYLINDRICAL_SURFACE('',#6543,2.475);
#414=CYLINDRICAL_SURFACE('',#6548,2.475);
#415=CYLINDRICAL_SURFACE('',#6562,5.);
#416=CYLINDRICAL_SURFACE('',#6574,35.);
#417=CYLINDRICAL_SURFACE('',#6578,40.);
#418=CYLINDRICAL_SURFACE('',#6582,35.);
#419=CYLINDRICAL_SURFACE('',#6594,5.);
#420=CYLINDRICAL_SURFACE('',#6598,2.5);
#421=CYLINDRICAL_SURFACE('',#6599,1.25);
#422=CYLINDRICAL_SURFACE('',#6600,1.25);
#423=CYLINDRICAL_SURFACE('',#6601,12.5);
#424=CYLINDRICAL_SURFACE('',#6602,12.5);
#425=CYLINDRICAL_SURFACE('',#6603,12.5);
#426=CYLINDRICAL_SURFACE('',#6604,12.5);
#427=CYLINDRICAL_SURFACE('',#6605,6.);
#428=CYLINDRICAL_SURFACE('',#6606,6.);
#429=CYLINDRICAL_SURFACE('',#6607,6.);
#430=CYLINDRICAL_SURFACE('',#6608,6.);
#431=CYLINDRICAL_SURFACE('',#6611,6.);
#432=CYLINDRICAL_SURFACE('',#6620,1.25);
#433=CYLINDRICAL_SURFACE('',#6628,0.3);
#434=CYLINDRICAL_SURFACE('',#6634,0.3);
#435=CYLINDRICAL_SURFACE('',#6638,3.5);
#436=CYLINDRICAL_SURFACE('',#6641,1.25);
#437=CYLINDRICAL_SURFACE('',#6642,1.25);
#438=CYLINDRICAL_SURFACE('',#6643,6.);
#439=CYLINDRICAL_SURFACE('',#6644,2.5);
#440=CYLINDRICAL_SURFACE('',#6647,1.5);
#441=CYLINDRICAL_SURFACE('',#6655,1.5);
#442=CYLINDRICAL_SURFACE('',#6659,2.);
#443=CYLINDRICAL_SURFACE('',#6663,3.5);
#444=CYLINDRICAL_SURFACE('',#6674,1.25);
#445=CYLINDRICAL_SURFACE('',#6682,2.5);
#446=CYLINDRICAL_SURFACE('',#6684,1.25);
#447=CYLINDRICAL_SURFACE('',#6686,1.25);
#448=CYLINDRICAL_SURFACE('',#6689,1.25);
#449=CYLINDRICAL_SURFACE('',#6691,1.25);
#450=CYLINDRICAL_SURFACE('',#6706,0.5);
#451=CYLINDRICAL_SURFACE('',#6713,1.75);
#452=CYLINDRICAL_SURFACE('',#6714,8.);
#453=CYLINDRICAL_SURFACE('',#6722,16.);
#454=CYLINDRICAL_SURFACE('',#6733,1.25);
#455=CYLINDRICAL_SURFACE('',#6734,1.25);
#456=CYLINDRICAL_SURFACE('',#6735,1.25);
#457=CYLINDRICAL_SURFACE('',#6740,10.5);
#458=CYLINDRICAL_SURFACE('',#6743,2.);
#459=CYLINDRICAL_SURFACE('',#6750,0.5);
#460=CYLINDRICAL_SURFACE('',#6753,2.);
#461=CYLINDRICAL_SURFACE('',#6756,1.5);
#462=CYLINDRICAL_SURFACE('',#6761,1.5);
#463=CYLINDRICAL_SURFACE('',#6766,1.5);
#464=CYLINDRICAL_SURFACE('',#6771,1.5);
#465=CYLINDRICAL_SURFACE('',#6776,1.75);
#466=CYLINDRICAL_SURFACE('',#6788,10.);
#467=CYLINDRICAL_SURFACE('',#6792,2.);
#468=CYLINDRICAL_SURFACE('',#6800,7.);
#469=CYLINDRICAL_SURFACE('',#6807,1.5);
#470=CYLINDRICAL_SURFACE('',#6808,1.5);
#471=CYLINDRICAL_SURFACE('',#6809,1.5);
#472=CYLINDRICAL_SURFACE('',#6814,16.);
#473=CYLINDRICAL_SURFACE('',#6821,1.75);
#474=CYLINDRICAL_SURFACE('',#6830,2.);
#475=CYLINDRICAL_SURFACE('',#6844,2.);
#476=CYLINDRICAL_SURFACE('',#6857,1.75);
#477=CYLINDRICAL_SURFACE('',#6861,3.5);
#478=CYLINDRICAL_SURFACE('',#6867,2.);
#479=CYLINDRICAL_SURFACE('',#6871,2.);
#480=CYLINDRICAL_SURFACE('',#6872,5.5);
#481=CYLINDRICAL_SURFACE('',#6873,2.);
#482=CYLINDRICAL_SURFACE('',#6874,2.);
#483=CYLINDRICAL_SURFACE('',#6875,5.5);
#484=CYLINDRICAL_SURFACE('',#6876,2.);
#485=CYLINDRICAL_SURFACE('',#6885,2.);
#486=CYLINDRICAL_SURFACE('',#6888,1.5);
#487=CYLINDRICAL_SURFACE('',#6891,1.25);
#488=CYLINDRICAL_SURFACE('',#6896,1.75);
#489=CYLINDRICAL_SURFACE('',#6905,1.25);
#490=CYLINDRICAL_SURFACE('',#6909,8.);
#491=CYLINDRICAL_SURFACE('',#6913,6.75);
#492=CYLINDRICAL_SURFACE('',#6917,8.);
#493=CYLINDRICAL_SURFACE('',#6918,1.5);
#494=CYLINDRICAL_SURFACE('',#6939,1.5);
#495=CYLINDRICAL_SURFACE('',#6947,1.);
#496=CYLINDRICAL_SURFACE('',#6957,2.);
#497=CYLINDRICAL_SURFACE('',#6959,2.);
#498=CYLINDRICAL_SURFACE('',#6961,2.);
#499=CYLINDRICAL_SURFACE('',#6963,2.);
#500=CYLINDRICAL_SURFACE('',#6966,1.);
#501=CYLINDRICAL_SURFACE('',#6968,1.);
#502=CYLINDRICAL_SURFACE('',#6970,1.);
#503=CYLINDRICAL_SURFACE('',#6972,1.5);
#504=FACE_BOUND('',#1372,.T.);
#505=FACE_BOUND('',#1373,.T.);
#506=FACE_BOUND('',#1377,.T.);
#507=FACE_BOUND('',#1378,.T.);
#508=FACE_BOUND('',#1379,.T.);
#509=FACE_BOUND('',#1380,.T.);
#510=FACE_BOUND('',#1384,.T.);
#511=FACE_BOUND('',#1385,.T.);
#512=FACE_BOUND('',#1386,.T.);
#513=FACE_BOUND('',#1387,.T.);
#514=FACE_BOUND('',#1397,.T.);
#515=FACE_BOUND('',#1398,.T.);
#516=FACE_BOUND('',#1399,.T.);
#517=FACE_BOUND('',#1400,.T.);
#518=FACE_BOUND('',#1401,.T.);
#519=FACE_BOUND('',#1402,.T.);
#520=FACE_BOUND('',#1405,.T.);
#521=FACE_BOUND('',#1406,.T.);
#522=FACE_BOUND('',#1407,.T.);
#523=FACE_BOUND('',#1408,.T.);
#524=FACE_BOUND('',#1409,.T.);
#525=FACE_BOUND('',#1410,.T.);
#526=FACE_BOUND('',#1434,.T.);
#527=FACE_BOUND('',#1437,.T.);
#528=FACE_BOUND('',#1439,.T.);
#529=FACE_BOUND('',#1443,.T.);
#530=FACE_BOUND('',#1445,.T.);
#531=FACE_BOUND('',#1447,.T.);
#532=FACE_BOUND('',#1451,.T.);
#533=FACE_BOUND('',#1478,.T.);
#534=FACE_BOUND('',#1485,.T.);
#535=FACE_BOUND('',#1494,.T.);
#536=FACE_BOUND('',#1499,.T.);
#537=FACE_BOUND('',#1501,.T.);
#538=FACE_BOUND('',#1502,.T.);
#539=FACE_BOUND('',#1506,.T.);
#540=FACE_BOUND('',#1511,.T.);
#541=FACE_BOUND('',#1530,.T.);
#542=FACE_BOUND('',#1531,.T.);
#543=FACE_BOUND('',#1557,.T.);
#544=FACE_BOUND('',#1560,.T.);
#545=FACE_BOUND('',#1562,.T.);
#546=FACE_BOUND('',#1570,.T.);
#547=FACE_BOUND('',#1574,.T.);
#548=FACE_BOUND('',#1577,.T.);
#549=FACE_BOUND('',#1580,.T.);
#550=FACE_BOUND('',#1583,.T.);
#551=FACE_BOUND('',#1585,.T.);
#552=FACE_BOUND('',#1587,.T.);
#553=FACE_BOUND('',#1588,.T.);
#554=FACE_BOUND('',#1590,.T.);
#555=FACE_BOUND('',#1591,.T.);
#556=FACE_BOUND('',#1592,.T.);
#557=FACE_BOUND('',#1593,.T.);
#558=FACE_BOUND('',#1594,.T.);
#559=FACE_BOUND('',#1595,.T.);
#560=FACE_BOUND('',#1596,.T.);
#561=FACE_BOUND('',#1597,.T.);
#562=FACE_BOUND('',#1598,.T.);
#563=FACE_BOUND('',#1601,.T.);
#564=FACE_BOUND('',#1604,.T.);
#565=FACE_BOUND('',#1607,.T.);
#566=FACE_BOUND('',#1608,.T.);
#567=FACE_BOUND('',#1609,.T.);
#568=FACE_BOUND('',#1610,.T.);
#569=FACE_BOUND('',#1611,.T.);
#570=FACE_BOUND('',#1612,.T.);
#571=FACE_BOUND('',#1613,.T.);
#572=FACE_BOUND('',#1614,.T.);
#573=FACE_BOUND('',#1615,.T.);
#574=FACE_BOUND('',#1618,.T.);
#575=FACE_BOUND('',#1620,.T.);
#576=FACE_BOUND('',#1621,.T.);
#577=FACE_BOUND('',#1634,.T.);
#578=FACE_BOUND('',#1635,.T.);
#579=FACE_BOUND('',#1638,.T.);
#580=FACE_BOUND('',#1651,.T.);
#581=FACE_BOUND('',#1653,.T.);
#582=FACE_BOUND('',#1656,.T.);
#583=FACE_BOUND('',#1660,.T.);
#584=FACE_BOUND('',#1663,.T.);
#585=FACE_BOUND('',#1672,.T.);
#586=FACE_BOUND('',#1675,.T.);
#587=FACE_BOUND('',#1676,.T.);
#588=FACE_BOUND('',#1689,.T.);
#589=FACE_BOUND('',#1690,.T.);
#590=FACE_BOUND('',#1693,.T.);
#591=FACE_BOUND('',#1694,.T.);
#592=FACE_BOUND('',#1696,.T.);
#593=FACE_BOUND('',#1697,.T.);
#594=FACE_BOUND('',#1698,.T.);
#595=FACE_BOUND('',#1699,.T.);
#596=FACE_BOUND('',#1703,.T.);
#597=FACE_BOUND('',#1704,.T.);
#598=FACE_BOUND('',#1705,.T.);
#599=FACE_BOUND('',#1706,.T.);
#600=FACE_BOUND('',#1712,.T.);
#601=FACE_BOUND('',#1725,.T.);
#602=FACE_BOUND('',#1728,.T.);
#603=FACE_BOUND('',#1731,.T.);
#604=FACE_BOUND('',#1734,.T.);
#605=FACE_BOUND('',#1737,.T.);
#606=FACE_BOUND('',#1739,.T.);
#607=FACE_BOUND('',#1740,.T.);
#608=FACE_BOUND('',#1741,.T.);
#609=FACE_BOUND('',#1742,.T.);
#610=FACE_BOUND('',#1745,.T.);
#611=FACE_BOUND('',#1748,.T.);
#612=FACE_BOUND('',#1752,.T.);
#613=FACE_BOUND('',#1753,.T.);
#614=FACE_BOUND('',#1754,.T.);
#615=FACE_BOUND('',#1755,.T.);
#616=FACE_BOUND('',#1770,.T.);
#617=FACE_BOUND('',#1773,.T.);
#618=FACE_BOUND('',#1782,.T.);
#619=FACE_BOUND('',#1790,.T.);
#620=FACE_BOUND('',#1794,.T.);
#621=FACE_BOUND('',#1797,.T.);
#622=FACE_BOUND('',#1806,.T.);
#623=FACE_BOUND('',#1808,.T.);
#624=FACE_BOUND('',#1815,.T.);
#625=FACE_BOUND('',#1818,.T.);
#626=FACE_BOUND('',#1820,.T.);
#627=FACE_BOUND('',#1823,.T.);
#628=FACE_BOUND('',#1826,.T.);
#629=FACE_BOUND('',#1829,.T.);
#630=FACE_BOUND('',#1833,.T.);
#631=FACE_BOUND('',#1835,.T.);
#632=FACE_BOUND('',#1836,.T.);
#633=FACE_BOUND('',#1839,.T.);
#634=FACE_BOUND('',#1840,.T.);
#635=FACE_BOUND('',#1843,.T.);
#636=CIRCLE('',#6215,1.5);
#637=CIRCLE('',#6216,1.5);
#638=CIRCLE('',#6220,2.5);
#639=CIRCLE('',#6221,2.5);
#640=CIRCLE('',#6222,2.5);
#641=CIRCLE('',#6223,2.5);
#642=CIRCLE('',#6227,2.5);
#643=CIRCLE('',#6228,2.5);
#644=CIRCLE('',#6229,2.5);
#645=CIRCLE('',#6230,2.5);
#646=CIRCLE('',#6236,1.5);
#647=CIRCLE('',#6239,1.5);
#648=CIRCLE('',#6244,10.);
#649=CIRCLE('',#6245,10.);
#650=CIRCLE('',#6246,10.);
#651=CIRCLE('',#6247,10.);
#652=CIRCLE('',#6248,2.5);
#653=CIRCLE('',#6249,2.5);
#654=CIRCLE('',#6250,2.5);
#655=CIRCLE('',#6251,1.75);
#656=CIRCLE('',#6252,1.75);
#657=CIRCLE('',#6253,2.5);
#658=CIRCLE('',#6255,2.5);
#659=CIRCLE('',#6257,8.);
#660=CIRCLE('',#6258,8.);
#661=CIRCLE('',#6259,8.);
#662=CIRCLE('',#6260,8.);
#663=CIRCLE('',#6261,2.5);
#664=CIRCLE('',#6262,2.5);
#665=CIRCLE('',#6263,2.5);
#666=CIRCLE('',#6264,1.75);
#667=CIRCLE('',#6265,1.75);
#668=CIRCLE('',#6272,10.);
#669=CIRCLE('',#6275,10.);
#670=CIRCLE('',#6278,10.);
#671=CIRCLE('',#6281,10.);
#672=CIRCLE('',#6292,2.);
#673=CIRCLE('',#6293,2.);
#674=CIRCLE('',#6295,1.75);
#675=CIRCLE('',#6297,2.);
#676=CIRCLE('',#6298,2.);
#677=CIRCLE('',#6300,1.75);
#678=CIRCLE('',#6303,4.5);
#679=CIRCLE('',#6305,4.5);
#680=CIRCLE('',#6306,4.5);
#681=CIRCLE('',#6308,0.5);
#682=CIRCLE('',#6309,4.);
#683=CIRCLE('',#6311,2.5);
#684=CIRCLE('',#6313,2.5);
#685=CIRCLE('',#6315,4.);
#686=CIRCLE('',#6317,0.5);
#687=CIRCLE('',#6318,4.5);
#688=CIRCLE('',#6319,4.5);
#689=CIRCLE('',#6321,4.5);
#690=CIRCLE('',#6324,1.);
#691=CIRCLE('',#6325,1.);
#692=CIRCLE('',#6328,1.);
#693=CIRCLE('',#6329,1.);
#694=CIRCLE('',#6331,1.);
#695=CIRCLE('',#6332,1.);
#696=CIRCLE('',#6334,1.);
#697=CIRCLE('',#6335,1.);
#698=CIRCLE('',#6337,1.);
#699=CIRCLE('',#6339,6.217106130074);
#700=CIRCLE('',#6340,6.217106130074);
#701=CIRCLE('',#6342,6.217106130074);
#702=CIRCLE('',#6344,3.);
#703=CIRCLE('',#6345,3.224413979295);
#704=CIRCLE('',#6346,3.224413979295);
#705=CIRCLE('',#6347,1.);
#706=CIRCLE('',#6348,1.);
#707=CIRCLE('',#6350,1.);
#708=CIRCLE('',#6353,1.);
#709=CIRCLE('',#6355,1.);
#710=CIRCLE('',#6356,1.);
#711=CIRCLE('',#6358,1.);
#712=CIRCLE('',#6360,1.);
#713=CIRCLE('',#6362,1.);
#714=CIRCLE('',#6365,1.);
#715=CIRCLE('',#6366,1.);
#716=CIRCLE('',#6368,1.);
#717=CIRCLE('',#6370,1.);
#718=CIRCLE('',#6372,1.);
#719=CIRCLE('',#6373,1.);
#720=CIRCLE('',#6376,1.);
#721=CIRCLE('',#6378,4.);
#722=CIRCLE('',#6380,1.);
#723=CIRCLE('',#6381,1.);
#724=CIRCLE('',#6384,1.);
#725=CIRCLE('',#6387,4.);
#726=CIRCLE('',#6389,1.5);
#727=CIRCLE('',#6391,1.25);
#728=CIRCLE('',#6394,6.712116818331);
#729=CIRCLE('',#6395,6.712116818331);
#730=CIRCLE('',#6397,7.150071143774);
#731=CIRCLE('',#6398,7.150071143774);
#732=CIRCLE('',#6399,7.110772629208);
#733=CIRCLE('',#6400,7.110772629208);
#734=CIRCLE('',#6402,3.);
#735=CIRCLE('',#6404,5.);
#736=CIRCLE('',#6405,12.13789139507);
#737=CIRCLE('',#6406,12.13789139507);
#738=CIRCLE('',#6407,12.13789139507);
#739=CIRCLE('',#6408,12.13789139507);
#740=CIRCLE('',#6409,1.);
#741=CIRCLE('',#6410,1.);
#742=CIRCLE('',#6412,2.);
#743=CIRCLE('',#6413,2.625);
#744=CIRCLE('',#6415,2.625);
#745=CIRCLE('',#6418,1.75);
#746=CIRCLE('',#6420,1.);
#747=CIRCLE('',#6421,1.);
#748=CIRCLE('',#6422,2.);
#749=CIRCLE('',#6424,1.75);
#750=CIRCLE('',#6427,2.625);
#751=CIRCLE('',#6428,2.625);
#752=CIRCLE('',#6430,2.);
#753=CIRCLE('',#6433,1.);
#754=CIRCLE('',#6434,1.);
#755=CIRCLE('',#6436,2.);
#756=CIRCLE('',#6437,1.);
#757=CIRCLE('',#6438,1.);
#758=CIRCLE('',#6440,2.);
#759=CIRCLE('',#6441,2.);
#760=CIRCLE('',#6444,1.);
#761=CIRCLE('',#6453,1.);
#762=CIRCLE('',#6454,1.);
#763=CIRCLE('',#6455,1.);
#764=CIRCLE('',#6460,1.);
#765=CIRCLE('',#6461,1.);
#766=CIRCLE('',#6463,1.);
#767=CIRCLE('',#6465,2.);
#768=CIRCLE('',#6466,2.);
#769=CIRCLE('',#6468,2.);
#770=CIRCLE('',#6470,1.);
#771=CIRCLE('',#6471,1.);
#772=CIRCLE('',#6472,1.);
#773=CIRCLE('',#6473,1.);
#774=CIRCLE('',#6474,2.);
#775=CIRCLE('',#6476,2.);
#776=CIRCLE('',#6479,1.);
#777=CIRCLE('',#6481,1.);
#778=CIRCLE('',#6482,1.);
#779=CIRCLE('',#6486,1.);
#780=CIRCLE('',#6488,1.);
#781=CIRCLE('',#6489,1.);
#782=CIRCLE('',#6491,1.);
#783=CIRCLE('',#6495,1.);
#784=CIRCLE('',#6498,1.);
#785=CIRCLE('',#6500,1.);
#786=CIRCLE('',#6501,1.);
#787=CIRCLE('',#6504,1.);
#788=CIRCLE('',#6506,1.);
#789=CIRCLE('',#6508,1.);
#790=CIRCLE('',#6514,3.);
#791=CIRCLE('',#6515,3.);
#792=CIRCLE('',#6517,2.625);
#793=CIRCLE('',#6519,3.);
#794=CIRCLE('',#6520,3.);
#795=CIRCLE('',#6522,2.625);
#796=CIRCLE('',#6525,2.75);
#797=CIRCLE('',#6533,2.75);
#798=CIRCLE('',#6535,2.75);
#799=CIRCLE('',#6537,2.75);
#800=CIRCLE('',#6539,1.75);
#801=CIRCLE('',#6541,1.75);
#802=CIRCLE('',#6544,2.475);
#803=CIRCLE('',#6545,2.475);
#804=CIRCLE('',#6547,2.75);
#805=CIRCLE('',#6549,2.475);
#806=CIRCLE('',#6550,2.475);
#807=CIRCLE('',#6552,2.75);
#808=CIRCLE('',#6560,5.);
#809=CIRCLE('',#6561,2.5);
#810=CIRCLE('',#6563,5.);
#811=CIRCLE('',#6565,35.);
#812=CIRCLE('',#6566,12.5);
#813=CIRCLE('',#6567,12.5);
#814=CIRCLE('',#6568,12.5);
#815=CIRCLE('',#6569,12.5);
#816=CIRCLE('',#6570,6.);
#817=CIRCLE('',#6571,6.);
#818=CIRCLE('',#6572,6.);
#819=CIRCLE('',#6573,6.);
#820=CIRCLE('',#6575,35.);
#821=CIRCLE('',#6577,40.);
#822=CIRCLE('',#6579,40.);
#823=CIRCLE('',#6581,35.);
#824=CIRCLE('',#6583,35.);
#825=CIRCLE('',#6585,5.);
#826=CIRCLE('',#6586,12.5);
#827=CIRCLE('',#6587,12.5);
#828=CIRCLE('',#6588,12.5);
#829=CIRCLE('',#6589,12.5);
#830=CIRCLE('',#6590,6.);
#831=CIRCLE('',#6591,6.);
#832=CIRCLE('',#6592,6.);
#833=CIRCLE('',#6593,6.);
#834=CIRCLE('',#6595,5.);
#835=CIRCLE('',#6597,2.5);
#836=CIRCLE('',#6612,6.);
#837=CIRCLE('',#6613,6.);
#838=CIRCLE('',#6614,6.);
#839=CIRCLE('',#6616,5.7);
#840=CIRCLE('',#6617,3.2);
#841=CIRCLE('',#6618,2.5);
#842=CIRCLE('',#6619,1.25);
#843=CIRCLE('',#6621,1.25);
#844=CIRCLE('',#6623,6.5);
#845=CIRCLE('',#6624,3.5);
#846=CIRCLE('',#6629,0.3);
#847=CIRCLE('',#6630,0.3);
#848=CIRCLE('',#6632,6.);
#849=CIRCLE('',#6633,0.3);
#850=CIRCLE('',#6635,0.3);
#851=CIRCLE('',#6637,3.5);
#852=CIRCLE('',#6645,2.5);
#853=CIRCLE('',#6648,1.5);
#854=CIRCLE('',#6649,1.5);
#855=CIRCLE('',#6651,1.25);
#856=CIRCLE('',#6654,1.5);
#857=CIRCLE('',#6656,1.5);
#858=CIRCLE('',#6658,2.);
#859=CIRCLE('',#6660,2.);
#860=CIRCLE('',#6662,3.5);
#861=CIRCLE('',#6664,3.5);
#862=CIRCLE('',#6665,3.5);
#863=CIRCLE('',#6666,3.5);
#864=CIRCLE('',#6667,3.5);
#865=CIRCLE('',#6668,3.5);
#866=CIRCLE('',#6675,1.25);
#867=CIRCLE('',#6676,1.25);
#868=CIRCLE('',#6678,1.5);
#869=CIRCLE('',#6681,2.5);
#870=CIRCLE('',#6683,2.5);
#871=CIRCLE('',#6685,1.25);
#872=CIRCLE('',#6687,1.25);
#873=CIRCLE('',#6690,1.25);
#874=CIRCLE('',#6692,1.25);
#875=CIRCLE('',#6705,10.);
#876=CIRCLE('',#6707,0.5);
#877=CIRCLE('',#6708,0.5);
#878=CIRCLE('',#6710,0.5);
#879=CIRCLE('',#6711,2.);
#880=CIRCLE('',#6712,1.75);
#881=CIRCLE('',#6715,8.);
#882=CIRCLE('',#6716,8.);
#883=CIRCLE('',#6718,16.);
#884=CIRCLE('',#6719,1.25);
#885=CIRCLE('',#6720,1.25);
#886=CIRCLE('',#6721,1.25);
#887=CIRCLE('',#6723,16.);
#888=CIRCLE('',#6724,16.);
#889=CIRCLE('',#6726,0.5);
#890=CIRCLE('',#6727,15.5);
#891=CIRCLE('',#6729,1.25);
#892=CIRCLE('',#6730,1.25);
#893=CIRCLE('',#6731,11.);
#894=CIRCLE('',#6732,1.25);
#895=CIRCLE('',#6737,0.5);
#896=CIRCLE('',#6738,10.5);
#897=CIRCLE('',#6739,10.5);
#898=CIRCLE('',#6741,10.4999999985);
#899=CIRCLE('',#6742,10.5);
#900=CIRCLE('',#6745,10.9999999985);
#901=CIRCLE('',#6749,0.5);
#902=CIRCLE('',#6754,2.);
#903=CIRCLE('',#6757,1.5);
#904=CIRCLE('',#6758,1.5);
#905=CIRCLE('',#6760,1.25);
#906=CIRCLE('',#6762,1.5);
#907=CIRCLE('',#6763,1.5);
#908=CIRCLE('',#6765,1.25);
#909=CIRCLE('',#6767,1.5);
#910=CIRCLE('',#6768,1.5);
#911=CIRCLE('',#6770,1.25);
#912=CIRCLE('',#6772,1.5);
#913=CIRCLE('',#6773,1.5);
#914=CIRCLE('',#6775,1.25);
#915=CIRCLE('',#6777,1.75);
#916=CIRCLE('',#6778,1.75);
#917=CIRCLE('',#6780,2.);
#918=CIRCLE('',#6783,16.);
#919=CIRCLE('',#6784,10.);
#920=CIRCLE('',#6785,1.5);
#921=CIRCLE('',#6786,1.5);
#922=CIRCLE('',#6787,1.5);
#923=CIRCLE('',#6789,10.);
#924=CIRCLE('',#6791,2.);
#925=CIRCLE('',#6793,2.);
#926=CIRCLE('',#6795,6.);
#927=CIRCLE('',#6797,1.);
#928=CIRCLE('',#6798,7.);
#929=CIRCLE('',#6799,7.);
#930=CIRCLE('',#6801,7.);
#931=CIRCLE('',#6803,15.5);
#932=CIRCLE('',#6804,1.5);
#933=CIRCLE('',#6805,1.5);
#934=CIRCLE('',#6806,1.5);
#935=CIRCLE('',#6811,0.5);
#936=CIRCLE('',#6812,16.);
#937=CIRCLE('',#6813,16.);
#938=CIRCLE('',#6820,1.75);
#939=CIRCLE('',#6822,1.75);
#940=CIRCLE('',#6831,2.);
#941=CIRCLE('',#6832,2.);
#942=CIRCLE('',#6834,1.75);
#943=CIRCLE('',#6838,2.);
#944=CIRCLE('',#6839,5.5);
#945=CIRCLE('',#6840,2.);
#946=CIRCLE('',#6841,2.);
#947=CIRCLE('',#6842,5.5);
#948=CIRCLE('',#6843,2.);
#949=CIRCLE('',#6845,2.);
#950=CIRCLE('',#6847,1.75);
#951=CIRCLE('',#6849,4.5);
#952=CIRCLE('',#6850,2.);
#953=CIRCLE('',#6851,5.5);
#954=CIRCLE('',#6853,2.);
#955=CIRCLE('',#6854,4.5);
#956=CIRCLE('',#6855,2.);
#957=CIRCLE('',#6856,5.5);
#958=CIRCLE('',#6858,1.75);
#959=CIRCLE('',#6860,3.5);
#960=CIRCLE('',#6862,3.5);
#961=CIRCLE('',#6863,3.5);
#962=CIRCLE('',#6866,2.);
#963=CIRCLE('',#6868,2.);
#964=CIRCLE('',#6877,2.);
#965=CIRCLE('',#6878,2.);
#966=CIRCLE('',#6880,1.75);
#967=CIRCLE('',#6883,2.);
#968=CIRCLE('',#6884,1.5);
#969=CIRCLE('',#6886,2.);
#970=CIRCLE('',#6889,1.5);
#971=CIRCLE('',#6892,1.25);
#972=CIRCLE('',#6893,1.25);
#973=CIRCLE('',#6895,1.5);
#974=CIRCLE('',#6897,1.75);
#975=CIRCLE('',#6898,1.75);
#976=CIRCLE('',#6900,2.);
#977=CIRCLE('',#6903,8.);
#978=CIRCLE('',#6904,1.25);
#979=CIRCLE('',#6906,1.25);
#980=CIRCLE('',#6908,8.);
#981=CIRCLE('',#6910,8.);
#982=CIRCLE('',#6912,6.75);
#983=CIRCLE('',#6914,6.75);
#984=CIRCLE('',#6916,8.);
#985=CIRCLE('',#6919,1.5);
#986=CIRCLE('',#6920,1.5);
#987=CIRCLE('',#6922,1.25);
#988=CIRCLE('',#6933,2.);
#989=CIRCLE('',#6934,2.);
#990=CIRCLE('',#6935,2.);
#991=CIRCLE('',#6936,2.);
#992=CIRCLE('',#6937,1.5);
#993=CIRCLE('',#6938,1.5);
#994=CIRCLE('',#6940,1.5);
#995=CIRCLE('',#6942,1.);
#996=CIRCLE('',#6943,1.);
#997=CIRCLE('',#6944,1.);
#998=CIRCLE('',#6945,1.);
#999=CIRCLE('',#6946,1.5);
#1000=CIRCLE('',#6948,1.);
#1001=CIRCLE('',#6950,2.);
#1002=CIRCLE('',#6951,2.);
#1003=CIRCLE('',#6952,2.);
#1004=CIRCLE('',#6953,2.);
#1005=CIRCLE('',#6954,1.);
#1006=CIRCLE('',#6955,1.);
#1007=CIRCLE('',#6956,1.);
#1008=FACE_OUTER_BOUND('',#1368,.T.);
#1009=FACE_OUTER_BOUND('',#1369,.T.);
#1010=FACE_OUTER_BOUND('',#1370,.T.);
#1011=FACE_OUTER_BOUND('',#1371,.T.);
#1012=FACE_OUTER_BOUND('',#1374,.T.);
#1013=FACE_OUTER_BOUND('',#1375,.T.);
#1014=FACE_OUTER_BOUND('',#1376,.T.);
#1015=FACE_OUTER_BOUND('',#1381,.T.);
#1016=FACE_OUTER_BOUND('',#1382,.T.);
#1017=FACE_OUTER_BOUND('',#1383,.T.);
#1018=FACE_OUTER_BOUND('',#1388,.T.);
#1019=FACE_OUTER_BOUND('',#1389,.T.);
#1020=FACE_OUTER_BOUND('',#1390,.T.);
#1021=FACE_OUTER_BOUND('',#1391,.T.);
#1022=FACE_OUTER_BOUND('',#1392,.T.);
#1023=FACE_OUTER_BOUND('',#1393,.T.);
#1024=FACE_OUTER_BOUND('',#1394,.T.);
#1025=FACE_OUTER_BOUND('',#1395,.T.);
#1026=FACE_OUTER_BOUND('',#1396,.T.);
#1027=FACE_OUTER_BOUND('',#1403,.T.);
#1028=FACE_OUTER_BOUND('',#1404,.T.);
#1029=FACE_OUTER_BOUND('',#1411,.T.);
#1030=FACE_OUTER_BOUND('',#1412,.T.);
#1031=FACE_OUTER_BOUND('',#1413,.T.);
#1032=FACE_OUTER_BOUND('',#1414,.T.);
#1033=FACE_OUTER_BOUND('',#1415,.T.);
#1034=FACE_OUTER_BOUND('',#1416,.T.);
#1035=FACE_OUTER_BOUND('',#1417,.T.);
#1036=FACE_OUTER_BOUND('',#1418,.T.);
#1037=FACE_OUTER_BOUND('',#1419,.T.);
#1038=FACE_OUTER_BOUND('',#1420,.T.);
#1039=FACE_OUTER_BOUND('',#1421,.T.);
#1040=FACE_OUTER_BOUND('',#1422,.T.);
#1041=FACE_OUTER_BOUND('',#1423,.T.);
#1042=FACE_OUTER_BOUND('',#1424,.T.);
#1043=FACE_OUTER_BOUND('',#1425,.T.);
#1044=FACE_OUTER_BOUND('',#1426,.T.);
#1045=FACE_OUTER_BOUND('',#1427,.T.);
#1046=FACE_OUTER_BOUND('',#1428,.T.);
#1047=FACE_OUTER_BOUND('',#1429,.T.);
#1048=FACE_OUTER_BOUND('',#1430,.T.);
#1049=FACE_OUTER_BOUND('',#1431,.T.);
#1050=FACE_OUTER_BOUND('',#1432,.T.);
#1051=FACE_OUTER_BOUND('',#1433,.T.);
#1052=FACE_OUTER_BOUND('',#1435,.T.);
#1053=FACE_OUTER_BOUND('',#1436,.T.);
#1054=FACE_OUTER_BOUND('',#1438,.T.);
#1055=FACE_OUTER_BOUND('',#1440,.T.);
#1056=FACE_OUTER_BOUND('',#1441,.T.);
#1057=FACE_OUTER_BOUND('',#1442,.T.);
#1058=FACE_OUTER_BOUND('',#1444,.T.);
#1059=FACE_OUTER_BOUND('',#1446,.T.);
#1060=FACE_OUTER_BOUND('',#1448,.T.);
#1061=FACE_OUTER_BOUND('',#1449,.T.);
#1062=FACE_OUTER_BOUND('',#1450,.T.);
#1063=FACE_OUTER_BOUND('',#1452,.T.);
#1064=FACE_OUTER_BOUND('',#1453,.T.);
#1065=FACE_OUTER_BOUND('',#1454,.T.);
#1066=FACE_OUTER_BOUND('',#1455,.T.);
#1067=FACE_OUTER_BOUND('',#1456,.T.);
#1068=FACE_OUTER_BOUND('',#1457,.T.);
#1069=FACE_OUTER_BOUND('',#1458,.T.);
#1070=FACE_OUTER_BOUND('',#1459,.T.);
#1071=FACE_OUTER_BOUND('',#1460,.T.);
#1072=FACE_OUTER_BOUND('',#1461,.T.);
#1073=FACE_OUTER_BOUND('',#1462,.T.);
#1074=FACE_OUTER_BOUND('',#1463,.T.);
#1075=FACE_OUTER_BOUND('',#1464,.T.);
#1076=FACE_OUTER_BOUND('',#1465,.T.);
#1077=FACE_OUTER_BOUND('',#1466,.T.);
#1078=FACE_OUTER_BOUND('',#1467,.T.);
#1079=FACE_OUTER_BOUND('',#1468,.T.);
#1080=FACE_OUTER_BOUND('',#1469,.T.);
#1081=FACE_OUTER_BOUND('',#1470,.T.);
#1082=FACE_OUTER_BOUND('',#1471,.T.);
#1083=FACE_OUTER_BOUND('',#1472,.T.);
#1084=FACE_OUTER_BOUND('',#1473,.T.);
#1085=FACE_OUTER_BOUND('',#1474,.T.);
#1086=FACE_OUTER_BOUND('',#1475,.T.);
#1087=FACE_OUTER_BOUND('',#1476,.T.);
#1088=FACE_OUTER_BOUND('',#1477,.T.);
#1089=FACE_OUTER_BOUND('',#1479,.T.);
#1090=FACE_OUTER_BOUND('',#1480,.T.);
#1091=FACE_OUTER_BOUND('',#1481,.T.);
#1092=FACE_OUTER_BOUND('',#1482,.T.);
#1093=FACE_OUTER_BOUND('',#1483,.T.);
#1094=FACE_OUTER_BOUND('',#1484,.T.);
#1095=FACE_OUTER_BOUND('',#1486,.T.);
#1096=FACE_OUTER_BOUND('',#1487,.T.);
#1097=FACE_OUTER_BOUND('',#1488,.T.);
#1098=FACE_OUTER_BOUND('',#1489,.T.);
#1099=FACE_OUTER_BOUND('',#1490,.T.);
#1100=FACE_OUTER_BOUND('',#1491,.T.);
#1101=FACE_OUTER_BOUND('',#1492,.T.);
#1102=FACE_OUTER_BOUND('',#1493,.T.);
#1103=FACE_OUTER_BOUND('',#1495,.T.);
#1104=FACE_OUTER_BOUND('',#1496,.T.);
#1105=FACE_OUTER_BOUND('',#1497,.T.);
#1106=FACE_OUTER_BOUND('',#1498,.T.);
#1107=FACE_OUTER_BOUND('',#1500,.T.);
#1108=FACE_OUTER_BOUND('',#1503,.T.);
#1109=FACE_OUTER_BOUND('',#1504,.T.);
#1110=FACE_OUTER_BOUND('',#1505,.T.);
#1111=FACE_OUTER_BOUND('',#1507,.T.);
#1112=FACE_OUTER_BOUND('',#1508,.T.);
#1113=FACE_OUTER_BOUND('',#1509,.T.);
#1114=FACE_OUTER_BOUND('',#1510,.T.);
#1115=FACE_OUTER_BOUND('',#1512,.T.);
#1116=FACE_OUTER_BOUND('',#1513,.T.);
#1117=FACE_OUTER_BOUND('',#1514,.T.);
#1118=FACE_OUTER_BOUND('',#1515,.T.);
#1119=FACE_OUTER_BOUND('',#1516,.T.);
#1120=FACE_OUTER_BOUND('',#1517,.T.);
#1121=FACE_OUTER_BOUND('',#1518,.T.);
#1122=FACE_OUTER_BOUND('',#1519,.T.);
#1123=FACE_OUTER_BOUND('',#1520,.T.);
#1124=FACE_OUTER_BOUND('',#1521,.T.);
#1125=FACE_OUTER_BOUND('',#1522,.T.);
#1126=FACE_OUTER_BOUND('',#1523,.T.);
#1127=FACE_OUTER_BOUND('',#1524,.T.);
#1128=FACE_OUTER_BOUND('',#1525,.T.);
#1129=FACE_OUTER_BOUND('',#1526,.T.);
#1130=FACE_OUTER_BOUND('',#1527,.T.);
#1131=FACE_OUTER_BOUND('',#1528,.T.);
#1132=FACE_OUTER_BOUND('',#1529,.T.);
#1133=FACE_OUTER_BOUND('',#1532,.T.);
#1134=FACE_OUTER_BOUND('',#1533,.T.);
#1135=FACE_OUTER_BOUND('',#1534,.T.);
#1136=FACE_OUTER_BOUND('',#1535,.T.);
#1137=FACE_OUTER_BOUND('',#1536,.T.);
#1138=FACE_OUTER_BOUND('',#1537,.T.);
#1139=FACE_OUTER_BOUND('',#1538,.T.);
#1140=FACE_OUTER_BOUND('',#1539,.T.);
#1141=FACE_OUTER_BOUND('',#1540,.T.);
#1142=FACE_OUTER_BOUND('',#1541,.T.);
#1143=FACE_OUTER_BOUND('',#1542,.T.);
#1144=FACE_OUTER_BOUND('',#1543,.T.);
#1145=FACE_OUTER_BOUND('',#1544,.T.);
#1146=FACE_OUTER_BOUND('',#1545,.T.);
#1147=FACE_OUTER_BOUND('',#1546,.T.);
#1148=FACE_OUTER_BOUND('',#1547,.T.);
#1149=FACE_OUTER_BOUND('',#1548,.T.);
#1150=FACE_OUTER_BOUND('',#1549,.T.);
#1151=FACE_OUTER_BOUND('',#1550,.T.);
#1152=FACE_OUTER_BOUND('',#1551,.T.);
#1153=FACE_OUTER_BOUND('',#1552,.T.);
#1154=FACE_OUTER_BOUND('',#1553,.T.);
#1155=FACE_OUTER_BOUND('',#1554,.T.);
#1156=FACE_OUTER_BOUND('',#1555,.T.);
#1157=FACE_OUTER_BOUND('',#1556,.T.);
#1158=FACE_OUTER_BOUND('',#1558,.T.);
#1159=FACE_OUTER_BOUND('',#1559,.T.);
#1160=FACE_OUTER_BOUND('',#1561,.T.);
#1161=FACE_OUTER_BOUND('',#1563,.T.);
#1162=FACE_OUTER_BOUND('',#1564,.T.);
#1163=FACE_OUTER_BOUND('',#1565,.T.);
#1164=FACE_OUTER_BOUND('',#1566,.T.);
#1165=FACE_OUTER_BOUND('',#1567,.T.);
#1166=FACE_OUTER_BOUND('',#1568,.T.);
#1167=FACE_OUTER_BOUND('',#1569,.T.);
#1168=FACE_OUTER_BOUND('',#1571,.T.);
#1169=FACE_OUTER_BOUND('',#1572,.T.);
#1170=FACE_OUTER_BOUND('',#1573,.T.);
#1171=FACE_OUTER_BOUND('',#1575,.T.);
#1172=FACE_OUTER_BOUND('',#1576,.T.);
#1173=FACE_OUTER_BOUND('',#1578,.T.);
#1174=FACE_OUTER_BOUND('',#1579,.T.);
#1175=FACE_OUTER_BOUND('',#1581,.T.);
#1176=FACE_OUTER_BOUND('',#1582,.T.);
#1177=FACE_OUTER_BOUND('',#1584,.T.);
#1178=FACE_OUTER_BOUND('',#1586,.T.);
#1179=FACE_OUTER_BOUND('',#1589,.T.);
#1180=FACE_OUTER_BOUND('',#1599,.T.);
#1181=FACE_OUTER_BOUND('',#1600,.T.);
#1182=FACE_OUTER_BOUND('',#1602,.T.);
#1183=FACE_OUTER_BOUND('',#1603,.T.);
#1184=FACE_OUTER_BOUND('',#1605,.T.);
#1185=FACE_OUTER_BOUND('',#1606,.T.);
#1186=FACE_OUTER_BOUND('',#1616,.T.);
#1187=FACE_OUTER_BOUND('',#1617,.T.);
#1188=FACE_OUTER_BOUND('',#1619,.T.);
#1189=FACE_OUTER_BOUND('',#1622,.T.);
#1190=FACE_OUTER_BOUND('',#1623,.T.);
#1191=FACE_OUTER_BOUND('',#1624,.T.);
#1192=FACE_OUTER_BOUND('',#1625,.T.);
#1193=FACE_OUTER_BOUND('',#1626,.T.);
#1194=FACE_OUTER_BOUND('',#1627,.T.);
#1195=FACE_OUTER_BOUND('',#1628,.T.);
#1196=FACE_OUTER_BOUND('',#1629,.T.);
#1197=FACE_OUTER_BOUND('',#1630,.T.);
#1198=FACE_OUTER_BOUND('',#1631,.T.);
#1199=FACE_OUTER_BOUND('',#1632,.T.);
#1200=FACE_OUTER_BOUND('',#1633,.T.);
#1201=FACE_OUTER_BOUND('',#1636,.T.);
#1202=FACE_OUTER_BOUND('',#1637,.T.);
#1203=FACE_OUTER_BOUND('',#1639,.T.);
#1204=FACE_OUTER_BOUND('',#1640,.T.);
#1205=FACE_OUTER_BOUND('',#1641,.T.);
#1206=FACE_OUTER_BOUND('',#1642,.T.);
#1207=FACE_OUTER_BOUND('',#1643,.T.);
#1208=FACE_OUTER_BOUND('',#1644,.T.);
#1209=FACE_OUTER_BOUND('',#1645,.T.);
#1210=FACE_OUTER_BOUND('',#1646,.T.);
#1211=FACE_OUTER_BOUND('',#1647,.T.);
#1212=FACE_OUTER_BOUND('',#1648,.T.);
#1213=FACE_OUTER_BOUND('',#1649,.T.);
#1214=FACE_OUTER_BOUND('',#1650,.T.);
#1215=FACE_OUTER_BOUND('',#1652,.T.);
#1216=FACE_OUTER_BOUND('',#1654,.T.);
#1217=FACE_OUTER_BOUND('',#1655,.T.);
#1218=FACE_OUTER_BOUND('',#1657,.T.);
#1219=FACE_OUTER_BOUND('',#1658,.T.);
#1220=FACE_OUTER_BOUND('',#1659,.T.);
#1221=FACE_OUTER_BOUND('',#1661,.T.);
#1222=FACE_OUTER_BOUND('',#1662,.T.);
#1223=FACE_OUTER_BOUND('',#1664,.T.);
#1224=FACE_OUTER_BOUND('',#1665,.T.);
#1225=FACE_OUTER_BOUND('',#1666,.T.);
#1226=FACE_OUTER_BOUND('',#1667,.T.);
#1227=FACE_OUTER_BOUND('',#1668,.T.);
#1228=FACE_OUTER_BOUND('',#1669,.T.);
#1229=FACE_OUTER_BOUND('',#1670,.T.);
#1230=FACE_OUTER_BOUND('',#1671,.T.);
#1231=FACE_OUTER_BOUND('',#1673,.T.);
#1232=FACE_OUTER_BOUND('',#1674,.T.);
#1233=FACE_OUTER_BOUND('',#1677,.T.);
#1234=FACE_OUTER_BOUND('',#1678,.T.);
#1235=FACE_OUTER_BOUND('',#1679,.T.);
#1236=FACE_OUTER_BOUND('',#1680,.T.);
#1237=FACE_OUTER_BOUND('',#1681,.T.);
#1238=FACE_OUTER_BOUND('',#1682,.T.);
#1239=FACE_OUTER_BOUND('',#1683,.T.);
#1240=FACE_OUTER_BOUND('',#1684,.T.);
#1241=FACE_OUTER_BOUND('',#1685,.T.);
#1242=FACE_OUTER_BOUND('',#1686,.T.);
#1243=FACE_OUTER_BOUND('',#1687,.T.);
#1244=FACE_OUTER_BOUND('',#1688,.T.);
#1245=FACE_OUTER_BOUND('',#1691,.T.);
#1246=FACE_OUTER_BOUND('',#1692,.T.);
#1247=FACE_OUTER_BOUND('',#1695,.T.);
#1248=FACE_OUTER_BOUND('',#1700,.T.);
#1249=FACE_OUTER_BOUND('',#1701,.T.);
#1250=FACE_OUTER_BOUND('',#1702,.T.);
#1251=FACE_OUTER_BOUND('',#1707,.T.);
#1252=FACE_OUTER_BOUND('',#1708,.T.);
#1253=FACE_OUTER_BOUND('',#1709,.T.);
#1254=FACE_OUTER_BOUND('',#1710,.T.);
#1255=FACE_OUTER_BOUND('',#1711,.T.);
#1256=FACE_OUTER_BOUND('',#1713,.T.);
#1257=FACE_OUTER_BOUND('',#1714,.T.);
#1258=FACE_OUTER_BOUND('',#1715,.T.);
#1259=FACE_OUTER_BOUND('',#1716,.T.);
#1260=FACE_OUTER_BOUND('',#1717,.T.);
#1261=FACE_OUTER_BOUND('',#1718,.T.);
#1262=FACE_OUTER_BOUND('',#1719,.T.);
#1263=FACE_OUTER_BOUND('',#1720,.T.);
#1264=FACE_OUTER_BOUND('',#1721,.T.);
#1265=FACE_OUTER_BOUND('',#1722,.T.);
#1266=FACE_OUTER_BOUND('',#1723,.T.);
#1267=FACE_OUTER_BOUND('',#1724,.T.);
#1268=FACE_OUTER_BOUND('',#1726,.T.);
#1269=FACE_OUTER_BOUND('',#1727,.T.);
#1270=FACE_OUTER_BOUND('',#1729,.T.);
#1271=FACE_OUTER_BOUND('',#1730,.T.);
#1272=FACE_OUTER_BOUND('',#1732,.T.);
#1273=FACE_OUTER_BOUND('',#1733,.T.);
#1274=FACE_OUTER_BOUND('',#1735,.T.);
#1275=FACE_OUTER_BOUND('',#1736,.T.);
#1276=FACE_OUTER_BOUND('',#1738,.T.);
#1277=FACE_OUTER_BOUND('',#1743,.T.);
#1278=FACE_OUTER_BOUND('',#1744,.T.);
#1279=FACE_OUTER_BOUND('',#1746,.T.);
#1280=FACE_OUTER_BOUND('',#1747,.T.);
#1281=FACE_OUTER_BOUND('',#1749,.T.);
#1282=FACE_OUTER_BOUND('',#1750,.T.);
#1283=FACE_OUTER_BOUND('',#1751,.T.);
#1284=FACE_OUTER_BOUND('',#1756,.T.);
#1285=FACE_OUTER_BOUND('',#1757,.T.);
#1286=FACE_OUTER_BOUND('',#1758,.T.);
#1287=FACE_OUTER_BOUND('',#1759,.T.);
#1288=FACE_OUTER_BOUND('',#1760,.T.);
#1289=FACE_OUTER_BOUND('',#1761,.T.);
#1290=FACE_OUTER_BOUND('',#1762,.T.);
#1291=FACE_OUTER_BOUND('',#1763,.T.);
#1292=FACE_OUTER_BOUND('',#1764,.T.);
#1293=FACE_OUTER_BOUND('',#1765,.T.);
#1294=FACE_OUTER_BOUND('',#1766,.T.);
#1295=FACE_OUTER_BOUND('',#1767,.T.);
#1296=FACE_OUTER_BOUND('',#1768,.T.);
#1297=FACE_OUTER_BOUND('',#1769,.T.);
#1298=FACE_OUTER_BOUND('',#1771,.T.);
#1299=FACE_OUTER_BOUND('',#1772,.T.);
#1300=FACE_OUTER_BOUND('',#1774,.T.);
#1301=FACE_OUTER_BOUND('',#1775,.T.);
#1302=FACE_OUTER_BOUND('',#1776,.T.);
#1303=FACE_OUTER_BOUND('',#1777,.T.);
#1304=FACE_OUTER_BOUND('',#1778,.T.);
#1305=FACE_OUTER_BOUND('',#1779,.T.);
#1306=FACE_OUTER_BOUND('',#1780,.T.);
#1307=FACE_OUTER_BOUND('',#1781,.T.);
#1308=FACE_OUTER_BOUND('',#1783,.T.);
#1309=FACE_OUTER_BOUND('',#1784,.T.);
#1310=FACE_OUTER_BOUND('',#1785,.T.);
#1311=FACE_OUTER_BOUND('',#1786,.T.);
#1312=FACE_OUTER_BOUND('',#1787,.T.);
#1313=FACE_OUTER_BOUND('',#1788,.T.);
#1314=FACE_OUTER_BOUND('',#1789,.T.);
#1315=FACE_OUTER_BOUND('',#1791,.T.);
#1316=FACE_OUTER_BOUND('',#1792,.T.);
#1317=FACE_OUTER_BOUND('',#1793,.T.);
#1318=FACE_OUTER_BOUND('',#1795,.T.);
#1319=FACE_OUTER_BOUND('',#1796,.T.);
#1320=FACE_OUTER_BOUND('',#1798,.T.);
#1321=FACE_OUTER_BOUND('',#1799,.T.);
#1322=FACE_OUTER_BOUND('',#1800,.T.);
#1323=FACE_OUTER_BOUND('',#1801,.T.);
#1324=FACE_OUTER_BOUND('',#1802,.T.);
#1325=FACE_OUTER_BOUND('',#1803,.T.);
#1326=FACE_OUTER_BOUND('',#1804,.T.);
#1327=FACE_OUTER_BOUND('',#1805,.T.);
#1328=FACE_OUTER_BOUND('',#1807,.T.);
#1329=FACE_OUTER_BOUND('',#1809,.T.);
#1330=FACE_OUTER_BOUND('',#1810,.T.);
#1331=FACE_OUTER_BOUND('',#1811,.T.);
#1332=FACE_OUTER_BOUND('',#1812,.T.);
#1333=FACE_OUTER_BOUND('',#1813,.T.);
#1334=FACE_OUTER_BOUND('',#1814,.T.);
#1335=FACE_OUTER_BOUND('',#1816,.T.);
#1336=FACE_OUTER_BOUND('',#1817,.T.);
#1337=FACE_OUTER_BOUND('',#1819,.T.);
#1338=FACE_OUTER_BOUND('',#1821,.T.);
#1339=FACE_OUTER_BOUND('',#1822,.T.);
#1340=FACE_OUTER_BOUND('',#1824,.T.);
#1341=FACE_OUTER_BOUND('',#1825,.T.);
#1342=FACE_OUTER_BOUND('',#1827,.T.);
#1343=FACE_OUTER_BOUND('',#1828,.T.);
#1344=FACE_OUTER_BOUND('',#1830,.T.);
#1345=FACE_OUTER_BOUND('',#1831,.T.);
#1346=FACE_OUTER_BOUND('',#1832,.T.);
#1347=FACE_OUTER_BOUND('',#1834,.T.);
#1348=FACE_OUTER_BOUND('',#1837,.T.);
#1349=FACE_OUTER_BOUND('',#1838,.T.);
#1350=FACE_OUTER_BOUND('',#1841,.T.);
#1351=FACE_OUTER_BOUND('',#1842,.T.);
#1352=FACE_OUTER_BOUND('',#1844,.T.);
#1353=FACE_OUTER_BOUND('',#1845,.T.);
#1354=FACE_OUTER_BOUND('',#1846,.T.);
#1355=FACE_OUTER_BOUND('',#1847,.T.);
#1356=FACE_OUTER_BOUND('',#1848,.T.);
#1357=FACE_OUTER_BOUND('',#1849,.T.);
#1358=FACE_OUTER_BOUND('',#1850,.T.);
#1359=FACE_OUTER_BOUND('',#1851,.T.);
#1360=FACE_OUTER_BOUND('',#1852,.T.);
#1361=FACE_OUTER_BOUND('',#1853,.T.);
#1362=FACE_OUTER_BOUND('',#1854,.T.);
#1363=FACE_OUTER_BOUND('',#1855,.T.);
#1364=FACE_OUTER_BOUND('',#1856,.T.);
#1365=FACE_OUTER_BOUND('',#1857,.T.);
#1366=FACE_OUTER_BOUND('',#1858,.T.);
#1367=FACE_OUTER_BOUND('',#1859,.T.);
#1368=EDGE_LOOP('',(#3916,#3917,#3918,#3919));
#1369=EDGE_LOOP('',(#3920,#3921,#3922,#3923));
#1370=EDGE_LOOP('',(#3924,#3925,#3926,#3927));
#1371=EDGE_LOOP('',(#3928,#3929,#3930,#3931,#3932,#3933));
#1372=EDGE_LOOP('',(#3934));
#1373=EDGE_LOOP('',(#3935));
#1374=EDGE_LOOP('',(#3936,#3937,#3938,#3939));
#1375=EDGE_LOOP('',(#3940,#3941,#3942,#3943,#3944));
#1376=EDGE_LOOP('',(#3945,#3946,#3947,#3948));
#1377=EDGE_LOOP('',(#3949));
#1378=EDGE_LOOP('',(#3950));
#1379=EDGE_LOOP('',(#3951));
#1380=EDGE_LOOP('',(#3952));
#1381=EDGE_LOOP('',(#3953,#3954,#3955,#3956,#3957));
#1382=EDGE_LOOP('',(#3958,#3959,#3960,#3961));
#1383=EDGE_LOOP('',(#3962,#3963,#3964,#3965));
#1384=EDGE_LOOP('',(#3966));
#1385=EDGE_LOOP('',(#3967));
#1386=EDGE_LOOP('',(#3968));
#1387=EDGE_LOOP('',(#3969));
#1388=EDGE_LOOP('',(#3970,#3971,#3972,#3973));
#1389=EDGE_LOOP('',(#3974,#3975,#3976,#3977));
#1390=EDGE_LOOP('',(#3978,#3979,#3980,#3981));
#1391=EDGE_LOOP('',(#3982,#3983,#3984,#3985));
#1392=EDGE_LOOP('',(#3986,#3987,#3988,#3989));
#1393=EDGE_LOOP('',(#3990));
#1394=EDGE_LOOP('',(#3991));
#1395=EDGE_LOOP('',(#3992,#3993,#3994,#3995));
#1396=EDGE_LOOP('',(#3996,#3997,#3998,#3999,#4000,#4001,#4002,#4003));
#1397=EDGE_LOOP('',(#4004));
#1398=EDGE_LOOP('',(#4005));
#1399=EDGE_LOOP('',(#4006));
#1400=EDGE_LOOP('',(#4007));
#1401=EDGE_LOOP('',(#4008));
#1402=EDGE_LOOP('',(#4009));
#1403=EDGE_LOOP('',(#4010,#4011,#4012,#4013));
#1404=EDGE_LOOP('',(#4014,#4015,#4016,#4017,#4018,#4019,#4020,#4021));
#1405=EDGE_LOOP('',(#4022));
#1406=EDGE_LOOP('',(#4023));
#1407=EDGE_LOOP('',(#4024));
#1408=EDGE_LOOP('',(#4025));
#1409=EDGE_LOOP('',(#4026));
#1410=EDGE_LOOP('',(#4027));
#1411=EDGE_LOOP('',(#4028,#4029,#4030,#4031));
#1412=EDGE_LOOP('',(#4032,#4033,#4034,#4035));
#1413=EDGE_LOOP('',(#4036,#4037,#4038,#4039));
#1414=EDGE_LOOP('',(#4040,#4041,#4042,#4043));
#1415=EDGE_LOOP('',(#4044,#4045,#4046,#4047));
#1416=EDGE_LOOP('',(#4048,#4049,#4050,#4051));
#1417=EDGE_LOOP('',(#4052,#4053,#4054,#4055));
#1418=EDGE_LOOP('',(#4056,#4057,#4058,#4059));
#1419=EDGE_LOOP('',(#4060,#4061,#4062,#4063));
#1420=EDGE_LOOP('',(#4064,#4065,#4066,#4067));
#1421=EDGE_LOOP('',(#4068,#4069,#4070,#4071));
#1422=EDGE_LOOP('',(#4072,#4073,#4074,#4075));
#1423=EDGE_LOOP('',(#4076,#4077,#4078,#4079));
#1424=EDGE_LOOP('',(#4080,#4081,#4082,#4083));
#1425=EDGE_LOOP('',(#4084,#4085,#4086,#4087));
#1426=EDGE_LOOP('',(#4088,#4089,#4090,#4091));
#1427=EDGE_LOOP('',(#4092,#4093,#4094,#4095));
#1428=EDGE_LOOP('',(#4096,#4097,#4098,#4099));
#1429=EDGE_LOOP('',(#4100,#4101,#4102,#4103));
#1430=EDGE_LOOP('',(#4104,#4105,#4106,#4107));
#1431=EDGE_LOOP('',(#4108,#4109,#4110,#4111));
#1432=EDGE_LOOP('',(#4112,#4113,#4114,#4115));
#1433=EDGE_LOOP('',(#4116));
#1434=EDGE_LOOP('',(#4117));
#1435=EDGE_LOOP('',(#4118,#4119,#4120,#4121));
#1436=EDGE_LOOP('',(#4122));
#1437=EDGE_LOOP('',(#4123));
#1438=EDGE_LOOP('',(#4124,#4125,#4126,#4127,#4128,#4129));
#1439=EDGE_LOOP('',(#4130));
#1440=EDGE_LOOP('',(#4131,#4132,#4133,#4134,#4135));
#1441=EDGE_LOOP('',(#4136,#4137,#4138,#4139,#4140));
#1442=EDGE_LOOP('',(#4141));
#1443=EDGE_LOOP('',(#4142));
#1444=EDGE_LOOP('',(#4143,#4144,#4145,#4146));
#1445=EDGE_LOOP('',(#4147,#4148));
#1446=EDGE_LOOP('',(#4149));
#1447=EDGE_LOOP('',(#4150));
#1448=EDGE_LOOP('',(#4151,#4152,#4153,#4154,#4155));
#1449=EDGE_LOOP('',(#4156,#4157,#4158,#4159,#4160));
#1450=EDGE_LOOP('',(#4161,#4162,#4163,#4164,#4165,#4166));
#1451=EDGE_LOOP('',(#4167));
#1452=EDGE_LOOP('',(#4168,#4169,#4170,#4171));
#1453=EDGE_LOOP('',(#4172,#4173,#4174,#4175));
#1454=EDGE_LOOP('',(#4176,#4177,#4178,#4179));
#1455=EDGE_LOOP('',(#4180,#4181,#4182));
#1456=EDGE_LOOP('',(#4183,#4184,#4185,#4186));
#1457=EDGE_LOOP('',(#4187,#4188,#4189,#4190));
#1458=EDGE_LOOP('',(#4191,#4192,#4193,#4194));
#1459=EDGE_LOOP('',(#4195,#4196,#4197,#4198,#4199));
#1460=EDGE_LOOP('',(#4200,#4201,#4202,#4203));
#1461=EDGE_LOOP('',(#4204,#4205,#4206,#4207,#4208,#4209,#4210,#4211,#4212));
#1462=EDGE_LOOP('',(#4213,#4214,#4215,#4216));
#1463=EDGE_LOOP('',(#4217,#4218,#4219,#4220));
#1464=EDGE_LOOP('',(#4221,#4222,#4223));
#1465=EDGE_LOOP('',(#4224,#4225,#4226,#4227));
#1466=EDGE_LOOP('',(#4228,#4229,#4230));
#1467=EDGE_LOOP('',(#4231,#4232,#4233,#4234));
#1468=EDGE_LOOP('',(#4235,#4236,#4237));
#1469=EDGE_LOOP('',(#4238,#4239,#4240,#4241));
#1470=EDGE_LOOP('',(#4242,#4243,#4244,#4245));
#1471=EDGE_LOOP('',(#4246,#4247,#4248,#4249));
#1472=EDGE_LOOP('',(#4250,#4251,#4252));
#1473=EDGE_LOOP('',(#4253,#4254,#4255,#4256));
#1474=EDGE_LOOP('',(#4257,#4258,#4259));
#1475=EDGE_LOOP('',(#4260,#4261,#4262,#4263));
#1476=EDGE_LOOP('',(#4264,#4265,#4266,#4267));
#1477=EDGE_LOOP('',(#4268,#4269,#4270,#4271));
#1478=EDGE_LOOP('',(#4272));
#1479=EDGE_LOOP('',(#4273,#4274,#4275,#4276));
#1480=EDGE_LOOP('',(#4277,#4278,#4279));
#1481=EDGE_LOOP('',(#4280,#4281,#4282));
#1482=EDGE_LOOP('',(#4283,#4284,#4285,#4286));
#1483=EDGE_LOOP('',(#4287,#4288,#4289,#4290));
#1484=EDGE_LOOP('',(#4291));
#1485=EDGE_LOOP('',(#4292));
#1486=EDGE_LOOP('',(#4293,#4294,#4295,#4296));
#1487=EDGE_LOOP('',(#4297,#4298,#4299,#4300,#4301));
#1488=EDGE_LOOP('',(#4302,#4303,#4304,#4305,#4306,#4307));
#1489=EDGE_LOOP('',(#4308,#4309,#4310,#4311,#4312,#4313));
#1490=EDGE_LOOP('',(#4314,#4315,#4316,#4317,#4318,#4319));
#1491=EDGE_LOOP('',(#4320,#4321,#4322,#4323,#4324,#4325,#4326,#4327,#4328,
#4329,#4330,#4331,#4332,#4333));
#1492=EDGE_LOOP('',(#4334,#4335,#4336,#4337));
#1493=EDGE_LOOP('',(#4338,#4339,#4340,#4341,#4342,#4343,#4344,#4345,#4346,
#4347,#4348));
#1494=EDGE_LOOP('',(#4349));
#1495=EDGE_LOOP('',(#4350,#4351,#4352,#4353,#4354,#4355,#4356,#4357,#4358));
#1496=EDGE_LOOP('',(#4359));
#1497=EDGE_LOOP('',(#4360,#4361,#4362,#4363,#4364,#4365));
#1498=EDGE_LOOP('',(#4366,#4367,#4368,#4369,#4370,#4371,#4372,#4373,#4374));
#1499=EDGE_LOOP('',(#4375));
#1500=EDGE_LOOP('',(#4376,#4377,#4378,#4379,#4380,#4381,#4382,#4383,#4384,
#4385));
#1501=EDGE_LOOP('',(#4386));
#1502=EDGE_LOOP('',(#4387));
#1503=EDGE_LOOP('',(#4388,#4389,#4390,#4391,#4392,#4393,#4394));
#1504=EDGE_LOOP('',(#4395,#4396,#4397,#4398,#4399,#4400,#4401,#4402,#4403,
#4404));
#1505=EDGE_LOOP('',(#4405,#4406,#4407,#4408,#4409,#4410,#4411,#4412,#4413,
#4414,#4415,#4416));
#1506=EDGE_LOOP('',(#4417));
#1507=EDGE_LOOP('',(#4418));
#1508=EDGE_LOOP('',(#4419,#4420,#4421,#4422,#4423));
#1509=EDGE_LOOP('',(#4424,#4425,#4426,#4427));
#1510=EDGE_LOOP('',(#4428,#4429,#4430,#4431,#4432,#4433,#4434,#4435,#4436,
#4437,#4438,#4439));
#1511=EDGE_LOOP('',(#4440));
#1512=EDGE_LOOP('',(#4441,#4442,#4443,#4444));
#1513=EDGE_LOOP('',(#4445,#4446,#4447,#4448));
#1514=EDGE_LOOP('',(#4449,#4450,#4451,#4452));
#1515=EDGE_LOOP('',(#4453,#4454,#4455));
#1516=EDGE_LOOP('',(#4456,#4457,#4458));
#1517=EDGE_LOOP('',(#4459,#4460,#4461));
#1518=EDGE_LOOP('',(#4462,#4463,#4464));
#1519=EDGE_LOOP('',(#4465,#4466,#4467,#4468));
#1520=EDGE_LOOP('',(#4469,#4470,#4471,#4472));
#1521=EDGE_LOOP('',(#4473,#4474,#4475,#4476));
#1522=EDGE_LOOP('',(#4477,#4478,#4479,#4480));
#1523=EDGE_LOOP('',(#4481,#4482,#4483,#4484));
#1524=EDGE_LOOP('',(#4485,#4486,#4487,#4488));
#1525=EDGE_LOOP('',(#4489,#4490,#4491,#4492));
#1526=EDGE_LOOP('',(#4493,#4494,#4495,#4496,#4497));
#1527=EDGE_LOOP('',(#4498,#4499,#4500,#4501,#4502,#4503,#4504));
#1528=EDGE_LOOP('',(#4505,#4506,#4507,#4508,#4509));
#1529=EDGE_LOOP('',(#4510,#4511,#4512,#4513,#4514,#4515,#4516,#4517));
#1530=EDGE_LOOP('',(#4518));
#1531=EDGE_LOOP('',(#4519));
#1532=EDGE_LOOP('',(#4520,#4521,#4522,#4523));
#1533=EDGE_LOOP('',(#4524,#4525,#4526,#4527,#4528,#4529));
#1534=EDGE_LOOP('',(#4530,#4531,#4532,#4533));
#1535=EDGE_LOOP('',(#4534,#4535,#4536));
#1536=EDGE_LOOP('',(#4537,#4538,#4539,#4540));
#1537=EDGE_LOOP('',(#4541,#4542,#4543,#4544));
#1538=EDGE_LOOP('',(#4545,#4546,#4547,#4548));
#1539=EDGE_LOOP('',(#4549,#4550,#4551));
#1540=EDGE_LOOP('',(#4552,#4553,#4554,#4555));
#1541=EDGE_LOOP('',(#4556,#4557,#4558,#4559));
#1542=EDGE_LOOP('',(#4560,#4561,#4562,#4563));
#1543=EDGE_LOOP('',(#4564,#4565,#4566,#4567));
#1544=EDGE_LOOP('',(#4568,#4569,#4570,#4571));
#1545=EDGE_LOOP('',(#4572,#4573,#4574,#4575));
#1546=EDGE_LOOP('',(#4576,#4577,#4578));
#1547=EDGE_LOOP('',(#4579,#4580,#4581,#4582));
#1548=EDGE_LOOP('',(#4583,#4584,#4585,#4586));
#1549=EDGE_LOOP('',(#4587,#4588,#4589));
#1550=EDGE_LOOP('',(#4590,#4591,#4592,#4593));
#1551=EDGE_LOOP('',(#4594,#4595,#4596,#4597));
#1552=EDGE_LOOP('',(#4598,#4599,#4600,#4601));
#1553=EDGE_LOOP('',(#4602,#4603,#4604,#4605));
#1554=EDGE_LOOP('',(#4606,#4607,#4608,#4609));
#1555=EDGE_LOOP('',(#4610,#4611,#4612,#4613));
#1556=EDGE_LOOP('',(#4614));
#1557=EDGE_LOOP('',(#4615));
#1558=EDGE_LOOP('',(#4616,#4617,#4618,#4619));
#1559=EDGE_LOOP('',(#4620));
#1560=EDGE_LOOP('',(#4621));
#1561=EDGE_LOOP('',(#4622,#4623,#4624,#4625,#4626,#4627));
#1562=EDGE_LOOP('',(#4628));
#1563=EDGE_LOOP('',(#4629,#4630,#4631,#4632));
#1564=EDGE_LOOP('',(#4633,#4634,#4635,#4636));
#1565=EDGE_LOOP('',(#4637,#4638,#4639,#4640));
#1566=EDGE_LOOP('',(#4641,#4642,#4643,#4644));
#1567=EDGE_LOOP('',(#4645,#4646,#4647,#4648));
#1568=EDGE_LOOP('',(#4649,#4650,#4651,#4652));
#1569=EDGE_LOOP('',(#4653,#4654,#4655,#4656,#4657,#4658));
#1570=EDGE_LOOP('',(#4659));
#1571=EDGE_LOOP('',(#4660,#4661,#4662,#4663));
#1572=EDGE_LOOP('',(#4664,#4665,#4666,#4667));
#1573=EDGE_LOOP('',(#4668));
#1574=EDGE_LOOP('',(#4669));
#1575=EDGE_LOOP('',(#4670,#4671,#4672,#4673));
#1576=EDGE_LOOP('',(#4674));
#1577=EDGE_LOOP('',(#4675));
#1578=EDGE_LOOP('',(#4676,#4677,#4678,#4679));
#1579=EDGE_LOOP('',(#4680));
#1580=EDGE_LOOP('',(#4681));
#1581=EDGE_LOOP('',(#4682,#4683,#4684,#4685));
#1582=EDGE_LOOP('',(#4686));
#1583=EDGE_LOOP('',(#4687));
#1584=EDGE_LOOP('',(#4688));
#1585=EDGE_LOOP('',(#4689));
#1586=EDGE_LOOP('',(#4690,#4691,#4692,#4693));
#1587=EDGE_LOOP('',(#4694,#4695));
#1588=EDGE_LOOP('',(#4696));
#1589=EDGE_LOOP('',(#4697));
#1590=EDGE_LOOP('',(#4698));
#1591=EDGE_LOOP('',(#4699));
#1592=EDGE_LOOP('',(#4700));
#1593=EDGE_LOOP('',(#4701));
#1594=EDGE_LOOP('',(#4702));
#1595=EDGE_LOOP('',(#4703));
#1596=EDGE_LOOP('',(#4704));
#1597=EDGE_LOOP('',(#4705));
#1598=EDGE_LOOP('',(#4706));
#1599=EDGE_LOOP('',(#4707,#4708,#4709,#4710));
#1600=EDGE_LOOP('',(#4711));
#1601=EDGE_LOOP('',(#4712));
#1602=EDGE_LOOP('',(#4713,#4714,#4715,#4716));
#1603=EDGE_LOOP('',(#4717));
#1604=EDGE_LOOP('',(#4718));
#1605=EDGE_LOOP('',(#4719,#4720,#4721,#4722));
#1606=EDGE_LOOP('',(#4723));
#1607=EDGE_LOOP('',(#4724));
#1608=EDGE_LOOP('',(#4725));
#1609=EDGE_LOOP('',(#4726));
#1610=EDGE_LOOP('',(#4727));
#1611=EDGE_LOOP('',(#4728));
#1612=EDGE_LOOP('',(#4729));
#1613=EDGE_LOOP('',(#4730));
#1614=EDGE_LOOP('',(#4731));
#1615=EDGE_LOOP('',(#4732));
#1616=EDGE_LOOP('',(#4733,#4734,#4735,#4736));
#1617=EDGE_LOOP('',(#4737));
#1618=EDGE_LOOP('',(#4738));
#1619=EDGE_LOOP('',(#4739,#4740,#4741,#4742));
#1620=EDGE_LOOP('',(#4743));
#1621=EDGE_LOOP('',(#4744,#4745));
#1622=EDGE_LOOP('',(#4746,#4747,#4748,#4749,#4750));
#1623=EDGE_LOOP('',(#4751,#4752,#4753,#4754,#4755));
#1624=EDGE_LOOP('',(#4756,#4757,#4758,#4759));
#1625=EDGE_LOOP('',(#4760,#4761,#4762,#4763));
#1626=EDGE_LOOP('',(#4764,#4765,#4766,#4767));
#1627=EDGE_LOOP('',(#4768,#4769,#4770,#4771));
#1628=EDGE_LOOP('',(#4772,#4773,#4774,#4775));
#1629=EDGE_LOOP('',(#4776,#4777,#4778,#4779));
#1630=EDGE_LOOP('',(#4780,#4781,#4782,#4783));
#1631=EDGE_LOOP('',(#4784,#4785,#4786,#4787));
#1632=EDGE_LOOP('',(#4788,#4789,#4790,#4791,#4792,#4793,#4794,#4795,#4796,
#4797,#4798));
#1633=EDGE_LOOP('',(#4799,#4800,#4801,#4802));
#1634=EDGE_LOOP('',(#4803));
#1635=EDGE_LOOP('',(#4804));
#1636=EDGE_LOOP('',(#4805,#4806,#4807,#4808));
#1637=EDGE_LOOP('',(#4809,#4810,#4811,#4812));
#1638=EDGE_LOOP('',(#4813));
#1639=EDGE_LOOP('',(#4814,#4815,#4816,#4817,#4818,#4819));
#1640=EDGE_LOOP('',(#4820,#4821,#4822,#4823,#4824,#4825));
#1641=EDGE_LOOP('',(#4826,#4827,#4828,#4829));
#1642=EDGE_LOOP('',(#4830,#4831,#4832,#4833,#4834));
#1643=EDGE_LOOP('',(#4835,#4836,#4837,#4838));
#1644=EDGE_LOOP('',(#4839,#4840,#4841,#4842));
#1645=EDGE_LOOP('',(#4843,#4844,#4845,#4846));
#1646=EDGE_LOOP('',(#4847,#4848,#4849,#4850,#4851,#4852));
#1647=EDGE_LOOP('',(#4853,#4854,#4855,#4856,#4857,#4858,#4859,#4860,#4861));
#1648=EDGE_LOOP('',(#4862,#4863,#4864,#4865,#4866,#4867,#4868,#4869));
#1649=EDGE_LOOP('',(#4870,#4871,#4872,#4873));
#1650=EDGE_LOOP('',(#4874,#4875,#4876,#4877,#4878,#4879,#4880,#4881));
#1651=EDGE_LOOP('',(#4882,#4883));
#1652=EDGE_LOOP('',(#4884));
#1653=EDGE_LOOP('',(#4885));
#1654=EDGE_LOOP('',(#4886,#4887,#4888,#4889));
#1655=EDGE_LOOP('',(#4890));
#1656=EDGE_LOOP('',(#4891));
#1657=EDGE_LOOP('',(#4892));
#1658=EDGE_LOOP('',(#4893,#4894,#4895,#4896));
#1659=EDGE_LOOP('',(#4897));
#1660=EDGE_LOOP('',(#4898));
#1661=EDGE_LOOP('',(#4899,#4900,#4901,#4902));
#1662=EDGE_LOOP('',(#4903));
#1663=EDGE_LOOP('',(#4904));
#1664=EDGE_LOOP('',(#4905,#4906,#4907,#4908,#4909,#4910,#4911,#4912,#4913,
#4914,#4915,#4916));
#1665=EDGE_LOOP('',(#4917,#4918,#4919,#4920));
#1666=EDGE_LOOP('',(#4921,#4922,#4923,#4924));
#1667=EDGE_LOOP('',(#4925,#4926,#4927,#4928));
#1668=EDGE_LOOP('',(#4929,#4930));
#1669=EDGE_LOOP('',(#4931,#4932,#4933));
#1670=EDGE_LOOP('',(#4934,#4935,#4936,#4937));
#1671=EDGE_LOOP('',(#4938));
#1672=EDGE_LOOP('',(#4939));
#1673=EDGE_LOOP('',(#4940));
#1674=EDGE_LOOP('',(#4941,#4942,#4943,#4944,#4945,#4946,#4947,#4948,#4949,
#4950,#4951,#4952));
#1675=EDGE_LOOP('',(#4953,#4954));
#1676=EDGE_LOOP('',(#4955));
#1677=EDGE_LOOP('',(#4956,#4957,#4958,#4959,#4960));
#1678=EDGE_LOOP('',(#4961,#4962,#4963,#4964,#4965));
#1679=EDGE_LOOP('',(#4966));
#1680=EDGE_LOOP('',(#4967,#4968,#4969,#4970,#4971));
#1681=EDGE_LOOP('',(#4972,#4973,#4974,#4975));
#1682=EDGE_LOOP('',(#4976));
#1683=EDGE_LOOP('',(#4977));
#1684=EDGE_LOOP('',(#4978));
#1685=EDGE_LOOP('',(#4979));
#1686=EDGE_LOOP('',(#4980,#4981,#4982,#4983));
#1687=EDGE_LOOP('',(#4984,#4985,#4986,#4987));
#1688=EDGE_LOOP('',(#4988,#4989,#4990,#4991,#4992,#4993));
#1689=EDGE_LOOP('',(#4994));
#1690=EDGE_LOOP('',(#4995));
#1691=EDGE_LOOP('',(#4996,#4997,#4998,#4999,#5000));
#1692=EDGE_LOOP('',(#5001,#5002,#5003,#5004));
#1693=EDGE_LOOP('',(#5005,#5006));
#1694=EDGE_LOOP('',(#5007,#5008));
#1695=EDGE_LOOP('',(#5009));
#1696=EDGE_LOOP('',(#5010));
#1697=EDGE_LOOP('',(#5011));
#1698=EDGE_LOOP('',(#5012));
#1699=EDGE_LOOP('',(#5013));
#1700=EDGE_LOOP('',(#5014,#5015,#5016,#5017,#5018));
#1701=EDGE_LOOP('',(#5019,#5020,#5021,#5022,#5023));
#1702=EDGE_LOOP('',(#5024));
#1703=EDGE_LOOP('',(#5025));
#1704=EDGE_LOOP('',(#5026));
#1705=EDGE_LOOP('',(#5027));
#1706=EDGE_LOOP('',(#5028));
#1707=EDGE_LOOP('',(#5029,#5030,#5031,#5032));
#1708=EDGE_LOOP('',(#5033,#5034,#5035,#5036));
#1709=EDGE_LOOP('',(#5037,#5038,#5039,#5040));
#1710=EDGE_LOOP('',(#5041,#5042,#5043,#5044,#5045));
#1711=EDGE_LOOP('',(#5046,#5047,#5048,#5049,#5050,#5051,#5052,#5053));
#1712=EDGE_LOOP('',(#5054));
#1713=EDGE_LOOP('',(#5055,#5056,#5057,#5058,#5059));
#1714=EDGE_LOOP('',(#5060,#5061,#5062,#5063));
#1715=EDGE_LOOP('',(#5064,#5065,#5066,#5067));
#1716=EDGE_LOOP('',(#5068,#5069,#5070,#5071,#5072));
#1717=EDGE_LOOP('',(#5073,#5074,#5075,#5076));
#1718=EDGE_LOOP('',(#5077,#5078,#5079,#5080));
#1719=EDGE_LOOP('',(#5081,#5082,#5083,#5084,#5085));
#1720=EDGE_LOOP('',(#5086));
#1721=EDGE_LOOP('',(#5087,#5088,#5089,#5090));
#1722=EDGE_LOOP('',(#5091));
#1723=EDGE_LOOP('',(#5092,#5093,#5094,#5095));
#1724=EDGE_LOOP('',(#5096));
#1725=EDGE_LOOP('',(#5097));
#1726=EDGE_LOOP('',(#5098,#5099,#5100,#5101));
#1727=EDGE_LOOP('',(#5102));
#1728=EDGE_LOOP('',(#5103));
#1729=EDGE_LOOP('',(#5104,#5105,#5106,#5107));
#1730=EDGE_LOOP('',(#5108));
#1731=EDGE_LOOP('',(#5109));
#1732=EDGE_LOOP('',(#5110,#5111,#5112,#5113));
#1733=EDGE_LOOP('',(#5114));
#1734=EDGE_LOOP('',(#5115));
#1735=EDGE_LOOP('',(#5116,#5117,#5118,#5119));
#1736=EDGE_LOOP('',(#5120));
#1737=EDGE_LOOP('',(#5121));
#1738=EDGE_LOOP('',(#5122));
#1739=EDGE_LOOP('',(#5123));
#1740=EDGE_LOOP('',(#5124));
#1741=EDGE_LOOP('',(#5125));
#1742=EDGE_LOOP('',(#5126));
#1743=EDGE_LOOP('',(#5127,#5128,#5129,#5130));
#1744=EDGE_LOOP('',(#5131));
#1745=EDGE_LOOP('',(#5132));
#1746=EDGE_LOOP('',(#5133,#5134,#5135,#5136));
#1747=EDGE_LOOP('',(#5137));
#1748=EDGE_LOOP('',(#5138));
#1749=EDGE_LOOP('',(#5139,#5140,#5141,#5142,#5143));
#1750=EDGE_LOOP('',(#5144,#5145,#5146,#5147,#5148));
#1751=EDGE_LOOP('',(#5149));
#1752=EDGE_LOOP('',(#5150));
#1753=EDGE_LOOP('',(#5151));
#1754=EDGE_LOOP('',(#5152));
#1755=EDGE_LOOP('',(#5153));
#1756=EDGE_LOOP('',(#5154,#5155,#5156,#5157));
#1757=EDGE_LOOP('',(#5158,#5159,#5160,#5161));
#1758=EDGE_LOOP('',(#5162,#5163,#5164,#5165));
#1759=EDGE_LOOP('',(#5166,#5167,#5168,#5169,#5170));
#1760=EDGE_LOOP('',(#5171,#5172,#5173,#5174,#5175));
#1761=EDGE_LOOP('',(#5176,#5177));
#1762=EDGE_LOOP('',(#5178,#5179,#5180,#5181));
#1763=EDGE_LOOP('',(#5182,#5183,#5184,#5185));
#1764=EDGE_LOOP('',(#5186,#5187,#5188,#5189));
#1765=EDGE_LOOP('',(#5190,#5191,#5192,#5193));
#1766=EDGE_LOOP('',(#5194,#5195,#5196,#5197));
#1767=EDGE_LOOP('',(#5198,#5199,#5200,#5201));
#1768=EDGE_LOOP('',(#5202,#5203));
#1769=EDGE_LOOP('',(#5204,#5205,#5206,#5207,#5208,#5209));
#1770=EDGE_LOOP('',(#5210));
#1771=EDGE_LOOP('',(#5211,#5212,#5213,#5214));
#1772=EDGE_LOOP('',(#5215,#5216,#5217,#5218,#5219,#5220));
#1773=EDGE_LOOP('',(#5221));
#1774=EDGE_LOOP('',(#5222,#5223,#5224,#5225));
#1775=EDGE_LOOP('',(#5226,#5227,#5228,#5229));
#1776=EDGE_LOOP('',(#5230,#5231,#5232,#5233));
#1777=EDGE_LOOP('',(#5234,#5235,#5236,#5237));
#1778=EDGE_LOOP('',(#5238,#5239,#5240,#5241));
#1779=EDGE_LOOP('',(#5242,#5243,#5244,#5245));
#1780=EDGE_LOOP('',(#5246,#5247,#5248,#5249));
#1781=EDGE_LOOP('',(#5250));
#1782=EDGE_LOOP('',(#5251));
#1783=EDGE_LOOP('',(#5252,#5253,#5254,#5255,#5256,#5257,#5258,#5259));
#1784=EDGE_LOOP('',(#5260,#5261,#5262,#5263));
#1785=EDGE_LOOP('',(#5264));
#1786=EDGE_LOOP('',(#5265,#5266,#5267,#5268,#5269,#5270));
#1787=EDGE_LOOP('',(#5271,#5272,#5273,#5274,#5275,#5276));
#1788=EDGE_LOOP('',(#5277,#5278,#5279,#5280));
#1789=EDGE_LOOP('',(#5281));
#1790=EDGE_LOOP('',(#5282));
#1791=EDGE_LOOP('',(#5283,#5284,#5285,#5286,#5287));
#1792=EDGE_LOOP('',(#5288,#5289,#5290,#5291));
#1793=EDGE_LOOP('',(#5292,#5293,#5294,#5295,#5296,#5297,#5298));
#1794=EDGE_LOOP('',(#5299));
#1795=EDGE_LOOP('',(#5300,#5301,#5302,#5303));
#1796=EDGE_LOOP('',(#5304,#5305,#5306,#5307,#5308,#5309,#5310));
#1797=EDGE_LOOP('',(#5311));
#1798=EDGE_LOOP('',(#5312,#5313,#5314,#5315));
#1799=EDGE_LOOP('',(#5316,#5317,#5318,#5319));
#1800=EDGE_LOOP('',(#5320,#5321,#5322,#5323));
#1801=EDGE_LOOP('',(#5324,#5325,#5326,#5327));
#1802=EDGE_LOOP('',(#5328,#5329,#5330,#5331));
#1803=EDGE_LOOP('',(#5332,#5333,#5334,#5335));
#1804=EDGE_LOOP('',(#5336,#5337,#5338,#5339));
#1805=EDGE_LOOP('',(#5340));
#1806=EDGE_LOOP('',(#5341));
#1807=EDGE_LOOP('',(#5342));
#1808=EDGE_LOOP('',(#5343));
#1809=EDGE_LOOP('',(#5344,#5345,#5346,#5347));
#1810=EDGE_LOOP('',(#5348));
#1811=EDGE_LOOP('',(#5349,#5350,#5351,#5352));
#1812=EDGE_LOOP('',(#5353));
#1813=EDGE_LOOP('',(#5354,#5355,#5356,#5357));
#1814=EDGE_LOOP('',(#5358));
#1815=EDGE_LOOP('',(#5359));
#1816=EDGE_LOOP('',(#5360,#5361,#5362,#5363));
#1817=EDGE_LOOP('',(#5364));
#1818=EDGE_LOOP('',(#5365));
#1819=EDGE_LOOP('',(#5366));
#1820=EDGE_LOOP('',(#5367));
#1821=EDGE_LOOP('',(#5368,#5369,#5370,#5371));
#1822=EDGE_LOOP('',(#5372));
#1823=EDGE_LOOP('',(#5373));
#1824=EDGE_LOOP('',(#5374,#5375,#5376,#5377));
#1825=EDGE_LOOP('',(#5378));
#1826=EDGE_LOOP('',(#5379));
#1827=EDGE_LOOP('',(#5380,#5381,#5382,#5383));
#1828=EDGE_LOOP('',(#5384));
#1829=EDGE_LOOP('',(#5385));
#1830=EDGE_LOOP('',(#5386,#5387,#5388,#5389));
#1831=EDGE_LOOP('',(#5390,#5391,#5392,#5393));
#1832=EDGE_LOOP('',(#5394));
#1833=EDGE_LOOP('',(#5395));
#1834=EDGE_LOOP('',(#5396,#5397,#5398,#5399,#5400,#5401,#5402,#5403));
#1835=EDGE_LOOP('',(#5404));
#1836=EDGE_LOOP('',(#5405));
#1837=EDGE_LOOP('',(#5406,#5407,#5408,#5409));
#1838=EDGE_LOOP('',(#5410,#5411,#5412,#5413,#5414,#5415,#5416,#5417));
#1839=EDGE_LOOP('',(#5418));
#1840=EDGE_LOOP('',(#5419));
#1841=EDGE_LOOP('',(#5420,#5421,#5422,#5423));
#1842=EDGE_LOOP('',(#5424,#5425,#5426,#5427,#5428,#5429,#5430,#5431));
#1843=EDGE_LOOP('',(#5432,#5433,#5434,#5435,#5436,#5437,#5438,#5439));
#1844=EDGE_LOOP('',(#5440,#5441,#5442,#5443));
#1845=EDGE_LOOP('',(#5444,#5445,#5446,#5447));
#1846=EDGE_LOOP('',(#5448,#5449,#5450,#5451));
#1847=EDGE_LOOP('',(#5452,#5453,#5454,#5455));
#1848=EDGE_LOOP('',(#5456,#5457,#5458,#5459));
#1849=EDGE_LOOP('',(#5460,#5461,#5462,#5463));
#1850=EDGE_LOOP('',(#5464,#5465,#5466,#5467));
#1851=EDGE_LOOP('',(#5468,#5469,#5470,#5471));
#1852=EDGE_LOOP('',(#5472,#5473,#5474,#5475));
#1853=EDGE_LOOP('',(#5476,#5477,#5478,#5479));
#1854=EDGE_LOOP('',(#5480,#5481,#5482,#5483));
#1855=EDGE_LOOP('',(#5484,#5485,#5486,#5487));
#1856=EDGE_LOOP('',(#5488,#5489,#5490,#5491));
#1857=EDGE_LOOP('',(#5492,#5493,#5494,#5495));
#1858=EDGE_LOOP('',(#5496,#5497,#5498,#5499));
#1859=EDGE_LOOP('',(#5500,#5501,#5502,#5503));
#1860=LINE('',#8882,#2221);
#1861=LINE('',#8884,#2222);
#1862=LINE('',#8886,#2223);
#1863=LINE('',#8887,#2224);
#1864=LINE('',#8890,#2225);
#1865=LINE('',#8892,#2226);
#1866=LINE('',#8893,#2227);
#1867=LINE('',#8897,#2228);
#1868=LINE('',#8898,#2229);
#1869=LINE('',#8899,#2230);
#1870=LINE('',#8903,#2231);
#1871=LINE('',#8904,#2232);
#1872=LINE('',#8906,#2233);
#1873=LINE('',#8908,#2234);
#1874=LINE('',#8909,#2235);
#1875=LINE('',#8916,#2236);
#1876=LINE('',#8918,#2237);
#1877=LINE('',#8919,#2238);
#1878=LINE('',#8921,#2239);
#1879=LINE('',#8923,#2240);
#1880=LINE('',#8933,#2241);
#1881=LINE('',#8935,#2242);
#1882=LINE('',#8946,#2243);
#1883=LINE('',#8948,#2244);
#1884=LINE('',#8950,#2245);
#1885=LINE('',#8952,#2246);
#1886=LINE('',#8956,#2247);
#1887=LINE('',#8962,#2248);
#1888=LINE('',#8970,#2249);
#1889=LINE('',#8974,#2250);
#1890=LINE('',#8978,#2251);
#1891=LINE('',#8981,#2252);
#1892=LINE('',#8996,#2253);
#1893=LINE('',#9003,#2254);
#1894=LINE('',#9007,#2255);
#1895=LINE('',#9011,#2256);
#1896=LINE('',#9014,#2257);
#1897=LINE('',#9026,#2258);
#1898=LINE('',#9028,#2259);
#1899=LINE('',#9030,#2260);
#1900=LINE('',#9032,#2261);
#1901=LINE('',#9034,#2262);
#1902=LINE('',#9037,#2263);
#1903=LINE('',#9040,#2264);
#1904=LINE('',#9043,#2265);
#1905=LINE('',#9044,#2266);
#1906=LINE('',#9048,#2267);
#1907=LINE('',#9051,#2268);
#1908=LINE('',#9052,#2269);
#1909=LINE('',#9056,#2270);
#1910=LINE('',#9059,#2271);
#1911=LINE('',#9060,#2272);
#1912=LINE('',#9064,#2273);
#1913=LINE('',#9066,#2274);
#1914=LINE('',#9068,#2275);
#1915=LINE('',#9069,#2276);
#1916=LINE('',#9071,#2277);
#1917=LINE('',#9073,#2278);
#1918=LINE('',#9075,#2279);
#1919=LINE('',#9077,#2280);
#1920=LINE('',#9079,#2281);
#1921=LINE('',#9081,#2282);
#1922=LINE('',#9087,#2283);
#1923=LINE('',#9096,#2284);
#1924=LINE('',#9105,#2285);
#1925=LINE('',#9107,#2286);
#1926=LINE('',#9109,#2287);
#1927=LINE('',#9123,#2288);
#1928=LINE('',#9124,#2289);
#1929=LINE('',#9129,#2290);
#1930=LINE('',#9142,#2291);
#1931=LINE('',#9193,#2292);
#1932=LINE('',#9198,#2293);
#1933=LINE('',#9200,#2294);
#1934=LINE('',#9202,#2295);
#1935=LINE('',#9204,#2296);
#1936=LINE('',#9217,#2297);
#1937=LINE('',#9221,#2298);
#1938=LINE('',#9226,#2299);
#1939=LINE('',#9228,#2300);
#1940=LINE('',#9229,#2301);
#1941=LINE('',#9234,#2302);
#1942=LINE('',#9241,#2303);
#1943=LINE('',#9348,#2304);
#1944=LINE('',#9352,#2305);
#1945=LINE('',#9360,#2306);
#1946=LINE('',#9361,#2307);
#1947=LINE('',#9488,#2308);
#1948=LINE('',#9494,#2309);
#1949=LINE('',#9498,#2310);
#1950=LINE('',#9499,#2311);
#1951=LINE('',#9504,#2312);
#1952=LINE('',#9510,#2313);
#1953=LINE('',#9518,#2314);
#1954=LINE('',#9521,#2315);
#1955=LINE('',#9534,#2316);
#1956=LINE('',#9541,#2317);
#1957=LINE('',#9543,#2318);
#1958=LINE('',#9548,#2319);
#1959=LINE('',#9556,#2320);
#1960=LINE('',#9880,#2321);
#1961=LINE('',#9882,#2322);
#1962=LINE('',#9884,#2323);
#1963=LINE('',#9886,#2324);
#1964=LINE('',#9890,#2325);
#1965=LINE('',#9892,#2326);
#1966=LINE('',#9894,#2327);
#1967=LINE('',#9896,#2328);
#1968=LINE('',#9897,#2329);
#1969=LINE('',#9902,#2330);
#1970=LINE('',#9935,#2331);
#1971=LINE('',#9958,#2332);
#1972=LINE('',#9964,#2333);
#1973=LINE('',#9966,#2334);
#1974=LINE('',#9969,#2335);
#1975=LINE('',#9970,#2336);
#1976=LINE('',#9976,#2337);
#1977=LINE('',#9977,#2338);
#1978=LINE('',#9986,#2339);
#1979=LINE('',#9988,#2340);
#1980=LINE('',#9990,#2341);
#1981=LINE('',#9992,#2342);
#1982=LINE('',#9994,#2343);
#1983=LINE('',#10029,#2344);
#1984=LINE('',#10061,#2345);
#1985=LINE('',#10063,#2346);
#1986=LINE('',#10068,#2347);
#1987=LINE('',#10070,#2348);
#1988=LINE('',#10072,#2349);
#1989=LINE('',#10095,#2350);
#1990=LINE('',#10097,#2351);
#1991=LINE('',#10099,#2352);
#1992=LINE('',#10100,#2353);
#1993=LINE('',#10107,#2354);
#1994=LINE('',#10109,#2355);
#1995=LINE('',#10120,#2356);
#1996=LINE('',#10121,#2357);
#1997=LINE('',#10123,#2358);
#1998=LINE('',#10124,#2359);
#1999=LINE('',#10126,#2360);
#2000=LINE('',#10128,#2361);
#2001=LINE('',#10130,#2362);
#2002=LINE('',#10132,#2363);
#2003=LINE('',#10134,#2364);
#2004=LINE('',#10139,#2365);
#2005=LINE('',#10144,#2366);
#2006=LINE('',#10146,#2367);
#2007=LINE('',#10149,#2368);
#2008=LINE('',#10151,#2369);
#2009=LINE('',#10262,#2370);
#2010=LINE('',#10264,#2371);
#2011=LINE('',#10270,#2372);
#2012=LINE('',#10272,#2373);
#2013=LINE('',#10273,#2374);
#2014=LINE('',#10278,#2375);
#2015=LINE('',#10283,#2376);
#2016=LINE('',#10288,#2377);
#2017=LINE('',#10293,#2378);
#2018=LINE('',#10297,#2379);
#2019=LINE('',#10299,#2380);
#2020=LINE('',#10300,#2381);
#2021=LINE('',#10308,#2382);
#2022=LINE('',#10311,#2383);
#2023=LINE('',#10312,#2384);
#2024=LINE('',#10325,#2385);
#2025=LINE('',#10328,#2386);
#2026=LINE('',#10329,#2387);
#2027=LINE('',#10344,#2388);
#2028=LINE('',#10346,#2389);
#2029=LINE('',#10352,#2390);
#2030=LINE('',#10361,#2391);
#2031=LINE('',#10370,#2392);
#2032=LINE('',#10372,#2393);
#2033=LINE('',#10374,#2394);
#2034=LINE('',#10376,#2395);
#2035=LINE('',#10378,#2396);
#2036=LINE('',#10379,#2397);
#2037=LINE('',#10384,#2398);
#2038=LINE('',#10386,#2399);
#2039=LINE('',#10387,#2400);
#2040=LINE('',#10390,#2401);
#2041=LINE('',#10391,#2402);
#2042=LINE('',#10394,#2403);
#2043=LINE('',#10395,#2404);
#2044=LINE('',#10398,#2405);
#2045=LINE('',#10399,#2406);
#2046=LINE('',#10402,#2407);
#2047=LINE('',#10403,#2408);
#2048=LINE('',#10405,#2409);
#2049=LINE('',#10411,#2410);
#2050=LINE('',#10416,#2411);
#2051=LINE('',#10422,#2412);
#2052=LINE('',#10429,#2413);
#2053=LINE('',#10438,#2414);
#2054=LINE('',#10456,#2415);
#2055=LINE('',#10553,#2416);
#2056=LINE('',#10560,#2417);
#2057=LINE('',#10567,#2418);
#2058=LINE('',#10590,#2419);
#2059=LINE('',#10596,#2420);
#2060=LINE('',#10672,#2421);
#2061=LINE('',#10674,#2422);
#2062=LINE('',#10676,#2423);
#2063=LINE('',#10678,#2424);
#2064=LINE('',#10680,#2425);
#2065=LINE('',#10682,#2426);
#2066=LINE('',#10684,#2427);
#2067=LINE('',#10686,#2428);
#2068=LINE('',#10688,#2429);
#2069=LINE('',#10690,#2430);
#2070=LINE('',#10697,#2431);
#2071=LINE('',#10747,#2432);
#2072=LINE('',#10751,#2433);
#2073=LINE('',#10776,#2434);
#2074=LINE('',#10779,#2435);
#2075=LINE('',#10786,#2436);
#2076=LINE('',#10793,#2437);
#2077=LINE('',#10796,#2438);
#2078=LINE('',#10823,#2439);
#2079=LINE('',#10824,#2440);
#2080=LINE('',#10827,#2441);
#2081=LINE('',#10836,#2442);
#2082=LINE('',#10841,#2443);
#2083=LINE('',#10852,#2444);
#2084=LINE('',#10931,#2445);
#2085=LINE('',#10934,#2446);
#2086=LINE('',#10936,#2447);
#2087=LINE('',#10943,#2448);
#2088=LINE('',#10954,#2449);
#2089=LINE('',#10961,#2450);
#2090=LINE('',#10968,#2451);
#2091=LINE('',#10972,#2452);
#2092=LINE('',#10976,#2453);
#2093=LINE('',#10980,#2454);
#2094=LINE('',#10984,#2455);
#2095=LINE('',#10987,#2456);
#2096=LINE('',#10988,#2457);
#2097=LINE('',#10990,#2458);
#2098=LINE('',#10992,#2459);
#2099=LINE('',#10999,#2460);
#2100=LINE('',#11012,#2461);
#2101=LINE('',#11033,#2462);
#2102=LINE('',#11053,#2463);
#2103=LINE('',#11169,#2464);
#2104=LINE('',#11172,#2465);
#2105=LINE('',#11177,#2466);
#2106=LINE('',#11182,#2467);
#2107=LINE('',#11197,#2468);
#2108=LINE('',#11199,#2469);
#2109=LINE('',#11201,#2470);
#2110=LINE('',#11208,#2471);
#2111=LINE('',#11211,#2472);
#2112=LINE('',#11213,#2473);
#2113=LINE('',#11215,#2474);
#2114=LINE('',#11260,#2475);
#2115=LINE('',#11265,#2476);
#2116=LINE('',#11316,#2477);
#2117=LINE('',#11334,#2478);
#2118=LINE('',#11336,#2479);
#2119=LINE('',#11338,#2480);
#2120=LINE('',#11347,#2481);
#2121=LINE('',#11350,#2482);
#2122=LINE('',#11353,#2483);
#2123=LINE('',#11390,#2484);
#2124=LINE('',#11404,#2485);
#2125=LINE('',#11405,#2486);
#2126=LINE('',#11410,#2487);
#2127=LINE('',#11416,#2488);
#2128=LINE('',#11422,#2489);
#2129=LINE('',#11431,#2490);
#2130=LINE('',#11440,#2491);
#2131=LINE('',#11449,#2492);
#2132=LINE('',#11458,#2493);
#2133=LINE('',#11477,#2494);
#2134=LINE('',#11484,#2495);
#2135=LINE('',#11497,#2496);
#2136=LINE('',#11509,#2497);
#2137=LINE('',#11511,#2498);
#2138=LINE('',#11513,#2499);
#2139=LINE('',#11521,#2500);
#2140=LINE('',#16711,#2501);
#2141=LINE('',#16713,#2502);
#2142=LINE('',#16715,#2503);
#2143=LINE('',#16717,#2504);
#2144=LINE('',#16719,#2505);
#2145=LINE('',#16720,#2506);
#2146=LINE('',#16725,#2507);
#2147=LINE('',#16730,#2508);
#2148=LINE('',#16732,#2509);
#2149=LINE('',#16734,#2510);
#2150=LINE('',#16736,#2511);
#2151=LINE('',#16738,#2512);
#2152=LINE('',#16739,#2513);
#2153=LINE('',#16741,#2514);
#2154=LINE('',#16742,#2515);
#2155=LINE('',#16744,#2516);
#2156=LINE('',#16746,#2517);
#2157=LINE('',#16748,#2518);
#2158=LINE('',#16750,#2519);
#2159=LINE('',#16756,#2520);
#2160=LINE('',#16772,#2521);
#2161=LINE('',#16779,#2522);
#2162=LINE('',#16784,#2523);
#2163=LINE('',#16785,#2524);
#2164=LINE('',#16791,#2525);
#2165=LINE('',#16795,#2526);
#2166=LINE('',#16804,#2527);
#2167=LINE('',#16808,#2528);
#2168=LINE('',#16814,#2529);
#2169=LINE('',#16821,#2530);
#2170=LINE('',#16835,#2531);
#2171=LINE('',#16840,#2532);
#2172=LINE('',#16845,#2533);
#2173=LINE('',#16848,#2534);
#2174=LINE('',#16855,#2535);
#2175=LINE('',#16857,#2536);
#2176=LINE('',#16860,#2537);
#2177=LINE('',#16866,#2538);
#2178=LINE('',#16880,#2539);
#2179=LINE('',#16885,#2540);
#2180=LINE('',#16891,#2541);
#2181=LINE('',#16900,#2542);
#2182=LINE('',#16913,#2543);
#2183=LINE('',#16920,#2544);
#2184=LINE('',#16927,#2545);
#2185=LINE('',#16933,#2546);
#2186=LINE('',#16938,#2547);
#2187=LINE('',#16957,#2548);
#2188=LINE('',#16961,#2549);
#2189=LINE('',#16965,#2550);
#2190=LINE('',#16968,#2551);
#2191=LINE('',#16975,#2552);
#2192=LINE('',#16982,#2553);
#2193=LINE('',#16986,#2554);
#2194=LINE('',#16990,#2555);
#2195=LINE('',#16993,#2556);
#2196=LINE('',#17000,#2557);
#2197=LINE('',#17001,#2558);
#2198=LINE('',#17007,#2559);
#2199=LINE('',#17011,#2560);
#2200=LINE('',#17015,#2561);
#2201=LINE('',#17018,#2562);
#2202=LINE('',#17020,#2563);
#2203=LINE('',#17024,#2564);
#2204=LINE('',#17028,#2565);
#2205=LINE('',#17031,#2566);
#2206=LINE('',#17033,#2567);
#2207=LINE('',#17034,#2568);
#2208=LINE('',#17036,#2569);
#2209=LINE('',#17038,#2570);
#2210=LINE('',#17040,#2571);
#2211=LINE('',#17042,#2572);
#2212=LINE('',#17044,#2573);
#2213=LINE('',#17046,#2574);
#2214=LINE('',#17049,#2575);
#2215=LINE('',#17051,#2576);
#2216=LINE('',#17053,#2577);
#2217=LINE('',#17055,#2578);
#2218=LINE('',#17057,#2579);
#2219=LINE('',#17059,#2580);
#2220=LINE('',#17062,#2581);
#2221=VECTOR('',#6984,100.);
#2222=VECTOR('',#6985,20.);
#2223=VECTOR('',#6986,100.);
#2224=VECTOR('',#6987,20.);
#2225=VECTOR('',#6990,8.66025403784361);
#2226=VECTOR('',#6991,90.);
#2227=VECTOR('',#6992,8.66025403784361);
#2228=VECTOR('',#6995,7.63762615826015);
#2229=VECTOR('',#6996,110.762395693);
#2230=VECTOR('',#6997,102.875644347);
#2231=VECTOR('',#7000,100.);
#2232=VECTOR('',#7001,18.4752086140694);
#2233=VECTOR('',#7002,90.);
#2234=VECTOR('',#7003,7.63762615826015);
#2235=VECTOR('',#7004,18.4752086140694);
#2236=VECTOR('',#7011,4.);
#2237=VECTOR('',#7012,100.);
#2238=VECTOR('',#7013,4.);
#2239=VECTOR('',#7016,120.);
#2240=VECTOR('',#7019,120.);
#2241=VECTOR('',#7030,110.762395693);
#2242=VECTOR('',#7033,102.875644347);
#2243=VECTOR('',#7046,2.5);
#2244=VECTOR('',#7049,2.5);
#2245=VECTOR('',#7052,2.5);
#2246=VECTOR('',#7055,2.5);
#2247=VECTOR('',#7060,1.5);
#2248=VECTOR('',#7069,1.5);
#2249=VECTOR('',#7078,65.);
#2250=VECTOR('',#7081,65.);
#2251=VECTOR('',#7084,65.);
#2252=VECTOR('',#7087,65.);
#2253=VECTOR('',#7102,2.5);
#2254=VECTOR('',#7109,64.99999997841);
#2255=VECTOR('',#7112,64.99999997841);
#2256=VECTOR('',#7115,64.99999997841);
#2257=VECTOR('',#7118,64.99999997841);
#2258=VECTOR('',#7131,2.5);
#2259=VECTOR('',#7134,2.5);
#2260=VECTOR('',#7137,2.5);
#2261=VECTOR('',#7140,1.75);
#2262=VECTOR('',#7143,1.75);
#2263=VECTOR('',#7146,2.82842712475481);
#2264=VECTOR('',#7149,2.82842712476101);
#2265=VECTOR('',#7152,64.99999997975);
#2266=VECTOR('',#7153,2.82842712475481);
#2267=VECTOR('',#7158,2.82842712476081);
#2268=VECTOR('',#7161,64.99999997975);
#2269=VECTOR('',#7162,2.82842712475481);
#2270=VECTOR('',#7167,2.82842712476101);
#2271=VECTOR('',#7170,64.99999997975);
#2272=VECTOR('',#7171,2.82842712475481);
#2273=VECTOR('',#7176,2.82842712476081);
#2274=VECTOR('',#7179,64.99999997975);
#2275=VECTOR('',#7182,4.000000000157);
#2276=VECTOR('',#7183,4.00000000009);
#2277=VECTOR('',#7186,4.000000000157);
#2278=VECTOR('',#7189,4.00000000009);
#2279=VECTOR('',#7192,4.000000000157);
#2280=VECTOR('',#7195,4.00000000009);
#2281=VECTOR('',#7198,4.000000000157);
#2282=VECTOR('',#7201,4.00000000009);
#2283=VECTOR('',#7208,2.);
#2284=VECTOR('',#7219,2.);
#2285=VECTOR('',#7230,14.);
#2286=VECTOR('',#7231,14.);
#2287=VECTOR('',#7232,5.371378300226);
#2288=VECTOR('',#7233,5.371378300181);
#2289=VECTOR('',#7234,14.);
#2290=VECTOR('',#7239,4.5);
#2291=VECTOR('',#7256,2.5);
#2292=VECTOR('',#7273,4.5);
#2293=VECTOR('',#7278,14.);
#2294=VECTOR('',#7279,14.);
#2295=VECTOR('',#7280,14.);
#2296=VECTOR('',#7281,5.371378300226);
#2297=VECTOR('',#7282,5.371378300181);
#2298=VECTOR('',#7285,14.);
#2299=VECTOR('',#7292,12.);
#2300=VECTOR('',#7293,14.);
#2301=VECTOR('',#7294,12.);
#2302=VECTOR('',#7299,12.);
#2303=VECTOR('',#7310,5.371378297288);
#2304=VECTOR('',#7317,5.371378302463);
#2305=VECTOR('',#7322,5.371378302463);
#2306=VECTOR('',#7331,5.371378297288);
#2307=VECTOR('',#7332,12.);
#2308=VECTOR('',#7363,12.);
#2309=VECTOR('',#7372,14.);
#2310=VECTOR('',#7377,14.);
#2311=VECTOR('',#7378,12.);
#2312=VECTOR('',#7383,12.);
#2313=VECTOR('',#7392,14.);
#2314=VECTOR('',#7405,12.);
#2315=VECTOR('',#7410,14.);
#2316=VECTOR('',#7431,4.);
#2317=VECTOR('',#7440,1.375);
#2318=VECTOR('',#7443,1.25);
#2319=VECTOR('',#7448,5.187242561534);
#2320=VECTOR('',#7457,5.187242561534);
#2321=VECTOR('',#7484,2.868878241544);
#2322=VECTOR('',#7485,1.868875965277);
#2323=VECTOR('',#7486,30.);
#2324=VECTOR('',#7487,14.);
#2325=VECTOR('',#7490,14.26794919243);
#2326=VECTOR('',#7491,1.);
#2327=VECTOR('',#7492,7.);
#2328=VECTOR('',#7493,1.);
#2329=VECTOR('',#7494,9.);
#2330=VECTOR('',#7499,2.625);
#2331=VECTOR('',#7500,2.625);
#2332=VECTOR('',#7507,1.75);
#2333=VECTOR('',#7514,24.);
#2334=VECTOR('',#7515,9.);
#2335=VECTOR('',#7518,10.);
#2336=VECTOR('',#7519,10.);
#2337=VECTOR('',#7524,14.26794919243);
#2338=VECTOR('',#7525,24.);
#2339=VECTOR('',#7526,7.);
#2340=VECTOR('',#7527,4.);
#2341=VECTOR('',#7528,40.);
#2342=VECTOR('',#7529,4.);
#2343=VECTOR('',#7530,7.);
#2344=VECTOR('',#7535,1.75);
#2345=VECTOR('',#7540,2.625);
#2346=VECTOR('',#7541,2.625);
#2347=VECTOR('',#7546,14.);
#2348=VECTOR('',#7547,30.);
#2349=VECTOR('',#7548,1.868878442791);
#2350=VECTOR('',#7549,2.868877901305);
#2351=VECTOR('',#7550,1.);
#2352=VECTOR('',#7551,7.);
#2353=VECTOR('',#7552,1.);
#2354=VECTOR('',#7561,7.);
#2355=VECTOR('',#7562,7.);
#2356=VECTOR('',#7575,31.);
#2357=VECTOR('',#7576,10.);
#2358=VECTOR('',#7577,10.);
#2359=VECTOR('',#7578,31.);
#2360=VECTOR('',#7579,7.);
#2361=VECTOR('',#7580,4.);
#2362=VECTOR('',#7581,40.);
#2363=VECTOR('',#7582,4.);
#2364=VECTOR('',#7583,7.);
#2365=VECTOR('',#7590,2.);
#2366=VECTOR('',#7599,2.868880399918);
#2367=VECTOR('',#7602,2.868878955581);
#2368=VECTOR('',#7607,2.868878761621);
#2369=VECTOR('',#7610,2.868878597225);
#2370=VECTOR('',#7635,7.);
#2371=VECTOR('',#7636,7.);
#2372=VECTOR('',#7643,7.);
#2373=VECTOR('',#7644,14.);
#2374=VECTOR('',#7645,7.);
#2375=VECTOR('',#7652,2.);
#2376=VECTOR('',#7657,14.);
#2377=VECTOR('',#7662,14.);
#2378=VECTOR('',#7669,2.);
#2379=VECTOR('',#7674,7.);
#2380=VECTOR('',#7675,14.);
#2381=VECTOR('',#7676,7.);
#2382=VECTOR('',#7689,4.);
#2383=VECTOR('',#7692,4.);
#2384=VECTOR('',#7693,14.);
#2385=VECTOR('',#7716,4.);
#2386=VECTOR('',#7719,14.);
#2387=VECTOR('',#7720,4.);
#2388=VECTOR('',#7749,24.);
#2389=VECTOR('',#7752,24.);
#2390=VECTOR('',#7759,3.);
#2391=VECTOR('',#7770,3.);
#2392=VECTOR('',#7781,4.618802153517);
#2393=VECTOR('',#7782,4.61880215351685);
#2394=VECTOR('',#7783,4.61880215351685);
#2395=VECTOR('',#7784,4.618802153517);
#2396=VECTOR('',#7785,4.61880215351685);
#2397=VECTOR('',#7786,4.61880215351685);
#2398=VECTOR('',#7791,2.);
#2399=VECTOR('',#7792,4.618802153517);
#2400=VECTOR('',#7793,2.);
#2401=VECTOR('',#7796,4.61880215351685);
#2402=VECTOR('',#7797,2.);
#2403=VECTOR('',#7800,4.61880215351685);
#2404=VECTOR('',#7801,2.);
#2405=VECTOR('',#7804,4.618802153517);
#2406=VECTOR('',#7805,2.);
#2407=VECTOR('',#7808,4.61880215351685);
#2408=VECTOR('',#7809,2.);
#2409=VECTOR('',#7812,4.61880215351685);
#2410=VECTOR('',#7819,2.75);
#2411=VECTOR('',#7826,2.75);
#2412=VECTOR('',#7833,1.75);
#2413=VECTOR('',#7842,2.475);
#2414=VECTOR('',#7853,2.475);
#2415=VECTOR('',#7880,5.);
#2416=VECTOR('',#7905,35.);
#2417=VECTOR('',#7914,40.);
#2418=VECTOR('',#7923,35.);
#2419=VECTOR('',#7948,5.);
#2420=VECTOR('',#7957,2.5);
#2421=VECTOR('',#7960,1.25);
#2422=VECTOR('',#7963,1.25);
#2423=VECTOR('',#7966,12.5);
#2424=VECTOR('',#7969,12.5);
#2425=VECTOR('',#7972,12.5);
#2426=VECTOR('',#7975,12.5);
#2427=VECTOR('',#7978,6.);
#2428=VECTOR('',#7981,6.);
#2429=VECTOR('',#7984,6.);
#2430=VECTOR('',#7987,6.);
#2431=VECTOR('',#7996,6.);
#2432=VECTOR('',#7999,3.268305009375);
#2433=VECTOR('',#8002,6.);
#2434=VECTOR('',#8007,17.82554346998);
#2435=VECTOR('',#8010,17.8255434699797);
#2436=VECTOR('',#8017,1.25);
#2437=VECTOR('',#8024,15.3255434699798);
#2438=VECTOR('',#8027,15.3255434699798);
#2439=VECTOR('',#8032,17.8255434887197);
#2440=VECTOR('',#8033,3.7);
#2441=VECTOR('',#8036,3.268305009375);
#2442=VECTOR('',#8051,17.8255434620497);
#2443=VECTOR('',#8060,3.7);
#2444=VECTOR('',#8067,1.25);
#2445=VECTOR('',#8070,1.25);
#2446=VECTOR('',#8075,2.5);
#2447=VECTOR('',#8076,2.5);
#2448=VECTOR('',#8085,1.5);
#2449=VECTOR('',#8100,1.5);
#2450=VECTOR('',#8109,2.);
#2451=VECTOR('',#8118,3.5);
#2452=VECTOR('',#8121,1.);
#2453=VECTOR('',#8124,1.);
#2454=VECTOR('',#8127,1.);
#2455=VECTOR('',#8130,1.);
#2456=VECTOR('',#8135,6.928203230276);
#2457=VECTOR('',#8136,6.928203230276);
#2458=VECTOR('',#8139,6.928203230276);
#2459=VECTOR('',#8142,6.928203230276);
#2460=VECTOR('',#8151,1.25);
#2461=VECTOR('',#8168,2.5);
#2462=VECTOR('',#8169,2.5);
#2463=VECTOR('',#8170,2.5);
#2464=VECTOR('',#8175,1.25);
#2465=VECTOR('',#8178,1.25);
#2466=VECTOR('',#8185,1.25);
#2467=VECTOR('',#8192,1.25);
#2468=VECTOR('',#8217,14.);
#2469=VECTOR('',#8218,20.);
#2470=VECTOR('',#8219,14.);
#2471=VECTOR('',#8228,13.99999999978);
#2472=VECTOR('',#8231,27.5);
#2473=VECTOR('',#8232,21.);
#2474=VECTOR('',#8233,27.5);
#2475=VECTOR('',#8242,1.75);
#2476=VECTOR('',#8247,8.);
#2477=VECTOR('',#8262,16.);
#2478=VECTOR('',#8285,1.25);
#2479=VECTOR('',#8288,1.25);
#2480=VECTOR('',#8291,1.25);
#2481=VECTOR('',#8302,10.5);
#2482=VECTOR('',#8305,28.);
#2483=VECTOR('',#8308,28.);
#2484=VECTOR('',#8311,2.);
#2485=VECTOR('',#8318,10.72128073786);
#2486=VECTOR('',#8319,10.72128073785);
#2487=VECTOR('',#8328,13.9999999992);
#2488=VECTOR('',#8337,2.);
#2489=VECTOR('',#8344,1.5);
#2490=VECTOR('',#8355,1.5);
#2491=VECTOR('',#8366,1.5);
#2492=VECTOR('',#8377,1.5);
#2493=VECTOR('',#8388,1.75);
#2494=VECTOR('',#8411,10.);
#2495=VECTOR('',#8420,2.);
#2496=VECTOR('',#8437,7.);
#2497=VECTOR('',#8452,1.5);
#2498=VECTOR('',#8455,1.5);
#2499=VECTOR('',#8458,1.5);
#2500=VECTOR('',#8469,16.);
#2501=VECTOR('',#8480,4.);
#2502=VECTOR('',#8481,3.99999999999987);
#2503=VECTOR('',#8482,3.99999999999987);
#2504=VECTOR('',#8483,4.);
#2505=VECTOR('',#8484,3.99999999999987);
#2506=VECTOR('',#8485,3.99999999999987);
#2507=VECTOR('',#8490,1.75);
#2508=VECTOR('',#8495,4.);
#2509=VECTOR('',#8496,3.99999999999987);
#2510=VECTOR('',#8497,3.99999999999987);
#2511=VECTOR('',#8498,4.);
#2512=VECTOR('',#8499,3.99999999999987);
#2513=VECTOR('',#8500,3.99999999999987);
#2514=VECTOR('',#8503,4.);
#2515=VECTOR('',#8504,4.);
#2516=VECTOR('',#8507,4.);
#2517=VECTOR('',#8510,4.);
#2518=VECTOR('',#8513,4.);
#2519=VECTOR('',#8516,4.);
#2520=VECTOR('',#8523,2.);
#2521=VECTOR('',#8542,6.324555320337);
#2522=VECTOR('',#8549,6.324555320337);
#2523=VECTOR('',#8554,13.);
#2524=VECTOR('',#8555,13.);
#2525=VECTOR('',#8562,10.);
#2526=VECTOR('',#8565,10.);
#2527=VECTOR('',#8574,10.);
#2528=VECTOR('',#8577,10.);
#2529=VECTOR('',#8584,1.75);
#2530=VECTOR('',#8593,3.5);
#2531=VECTOR('',#8602,13.);
#2532=VECTOR('',#8603,13.);
#2533=VECTOR('',#8608,2.);
#2534=VECTOR('',#8613,13.);
#2535=VECTOR('',#8618,13.);
#2536=VECTOR('',#8621,13.);
#2537=VECTOR('',#8626,13.);
#2538=VECTOR('',#8633,2.);
#2539=VECTOR('',#8652,2.);
#2540=VECTOR('',#8659,1.5);
#2541=VECTOR('',#8666,1.25);
#2542=VECTOR('',#8677,1.75);
#2543=VECTOR('',#8694,1.25);
#2544=VECTOR('',#8703,8.);
#2545=VECTOR('',#8712,6.75);
#2546=VECTOR('',#8721,8.);
#2547=VECTOR('',#8726,1.5);
#2548=VECTOR('',#8755,58.);
#2549=VECTOR('',#8758,6.);
#2550=VECTOR('',#8761,58.);
#2551=VECTOR('',#8764,6.);
#2552=VECTOR('',#8771,1.5);
#2553=VECTOR('',#8778,6.);
#2554=VECTOR('',#8781,58.);
#2555=VECTOR('',#8784,6.);
#2556=VECTOR('',#8787,58.);
#2557=VECTOR('',#8794,0.5);
#2558=VECTOR('',#8795,0.5);
#2559=VECTOR('',#8800,6.);
#2560=VECTOR('',#8803,58.);
#2561=VECTOR('',#8806,6.);
#2562=VECTOR('',#8809,58.);
#2563=VECTOR('',#8810,58.);
#2564=VECTOR('',#8813,6.);
#2565=VECTOR('',#8816,58.);
#2566=VECTOR('',#8819,6.);
#2567=VECTOR('',#8822,1.);
#2568=VECTOR('',#8823,1.);
#2569=VECTOR('',#8826,1.);
#2570=VECTOR('',#8829,1.);
#2571=VECTOR('',#8832,1.);
#2572=VECTOR('',#8835,1.);
#2573=VECTOR('',#8838,1.);
#2574=VECTOR('',#8841,1.);
#2575=VECTOR('',#8846,0.5);
#2576=VECTOR('',#8849,0.5);
#2577=VECTOR('',#8852,0.5);
#2578=VECTOR('',#8855,0.5);
#2579=VECTOR('',#8858,0.5);
#2580=VECTOR('',#8861,0.5);
#2581=VECTOR('',#8866,1.5);
#2582=VERTEX_POINT('',#8880);
#2583=VERTEX_POINT('',#8881);
#2584=VERTEX_POINT('',#8883);
#2585=VERTEX_POINT('',#8885);
#2586=VERTEX_POINT('',#8889);
#2587=VERTEX_POINT('',#8891);
#2588=VERTEX_POINT('',#8895);
#2589=VERTEX_POINT('',#8896);
#2590=VERTEX_POINT('',#8901);
#2591=VERTEX_POINT('',#8902);
#2592=VERTEX_POINT('',#8905);
#2593=VERTEX_POINT('',#8907);
#2594=VERTEX_POINT('',#8910);
#2595=VERTEX_POINT('',#8912);
#2596=VERTEX_POINT('',#8915);
#2597=VERTEX_POINT('',#8917);
#2598=VERTEX_POINT('',#8924);
#2599=VERTEX_POINT('',#8926);
#2600=VERTEX_POINT('',#8928);
#2601=VERTEX_POINT('',#8930);
#2602=VERTEX_POINT('',#8937);
#2603=VERTEX_POINT('',#8939);
#2604=VERTEX_POINT('',#8941);
#2605=VERTEX_POINT('',#8943);
#2606=VERTEX_POINT('',#8954);
#2607=VERTEX_POINT('',#8959);
#2608=VERTEX_POINT('',#8966);
#2609=VERTEX_POINT('',#8967);
#2610=VERTEX_POINT('',#8969);
#2611=VERTEX_POINT('',#8971);
#2612=VERTEX_POINT('',#8973);
#2613=VERTEX_POINT('',#8975);
#2614=VERTEX_POINT('',#8977);
#2615=VERTEX_POINT('',#8979);
#2616=VERTEX_POINT('',#8982);
#2617=VERTEX_POINT('',#8984);
#2618=VERTEX_POINT('',#8986);
#2619=VERTEX_POINT('',#8988);
#2620=VERTEX_POINT('',#8990);
#2621=VERTEX_POINT('',#8992);
#2622=VERTEX_POINT('',#8995);
#2623=VERTEX_POINT('',#8999);
#2624=VERTEX_POINT('',#9000);
#2625=VERTEX_POINT('',#9002);
#2626=VERTEX_POINT('',#9004);
#2627=VERTEX_POINT('',#9006);
#2628=VERTEX_POINT('',#9008);
#2629=VERTEX_POINT('',#9010);
#2630=VERTEX_POINT('',#9012);
#2631=VERTEX_POINT('',#9015);
#2632=VERTEX_POINT('',#9017);
#2633=VERTEX_POINT('',#9019);
#2634=VERTEX_POINT('',#9021);
#2635=VERTEX_POINT('',#9023);
#2636=VERTEX_POINT('',#9036);
#2637=VERTEX_POINT('',#9038);
#2638=VERTEX_POINT('',#9042);
#2639=VERTEX_POINT('',#9046);
#2640=VERTEX_POINT('',#9050);
#2641=VERTEX_POINT('',#9054);
#2642=VERTEX_POINT('',#9058);
#2643=VERTEX_POINT('',#9062);
#2644=VERTEX_POINT('',#9084);
#2645=VERTEX_POINT('',#9086);
#2646=VERTEX_POINT('',#9090);
#2647=VERTEX_POINT('',#9093);
#2648=VERTEX_POINT('',#9095);
#2649=VERTEX_POINT('',#9099);
#2650=VERTEX_POINT('',#9103);
#2651=VERTEX_POINT('',#9104);
#2652=VERTEX_POINT('',#9106);
#2653=VERTEX_POINT('',#9108);
#2654=VERTEX_POINT('',#9110);
#2655=VERTEX_POINT('',#9122);
#2656=VERTEX_POINT('',#9125);
#2657=VERTEX_POINT('',#9128);
#2658=VERTEX_POINT('',#9130);
#2659=VERTEX_POINT('',#9134);
#2660=VERTEX_POINT('',#9138);
#2661=VERTEX_POINT('',#9141);
#2662=VERTEX_POINT('',#9144);
#2663=VERTEX_POINT('',#9145);
#2664=VERTEX_POINT('',#9183);
#2665=VERTEX_POINT('',#9186);
#2666=VERTEX_POINT('',#9188);
#2667=VERTEX_POINT('',#9192);
#2668=VERTEX_POINT('',#9196);
#2669=VERTEX_POINT('',#9197);
#2670=VERTEX_POINT('',#9199);
#2671=VERTEX_POINT('',#9201);
#2672=VERTEX_POINT('',#9203);
#2673=VERTEX_POINT('',#9205);
#2674=VERTEX_POINT('',#9219);
#2675=VERTEX_POINT('',#9220);
#2676=VERTEX_POINT('',#9225);
#2677=VERTEX_POINT('',#9227);
#2678=VERTEX_POINT('',#9231);
#2679=VERTEX_POINT('',#9233);
#2680=VERTEX_POINT('',#9240);
#2681=VERTEX_POINT('',#9295);
#2682=VERTEX_POINT('',#9347);
#2683=VERTEX_POINT('',#9351);
#2684=VERTEX_POINT('',#9353);
#2685=VERTEX_POINT('',#9357);
#2686=VERTEX_POINT('',#9359);
#2687=VERTEX_POINT('',#9363);
#2688=VERTEX_POINT('',#9365);
#2689=VERTEX_POINT('',#9483);
#2690=VERTEX_POINT('',#9487);
#2691=VERTEX_POINT('',#9493);
#2692=VERTEX_POINT('',#9497);
#2693=VERTEX_POINT('',#9501);
#2694=VERTEX_POINT('',#9503);
#2695=VERTEX_POINT('',#9509);
#2696=VERTEX_POINT('',#9517);
#2697=VERTEX_POINT('',#9522);
#2698=VERTEX_POINT('',#9532);
#2699=VERTEX_POINT('',#9536);
#2700=VERTEX_POINT('',#9539);
#2701=VERTEX_POINT('',#9545);
#2702=VERTEX_POINT('',#9546);
#2703=VERTEX_POINT('',#9551);
#2704=VERTEX_POINT('',#9552);
#2705=VERTEX_POINT('',#9555);
#2706=VERTEX_POINT('',#9557);
#2707=VERTEX_POINT('',#9563);
#2708=VERTEX_POINT('',#9565);
#2709=VERTEX_POINT('',#9576);
#2710=VERTEX_POINT('',#9578);
#2711=VERTEX_POINT('',#9622);
#2712=VERTEX_POINT('',#9669);
#2713=VERTEX_POINT('',#9671);
#2714=VERTEX_POINT('',#9691);
#2715=VERTEX_POINT('',#9693);
#2716=VERTEX_POINT('',#9776);
#2717=VERTEX_POINT('',#9859);
#2718=VERTEX_POINT('',#9860);
#2719=VERTEX_POINT('',#9879);
#2720=VERTEX_POINT('',#9881);
#2721=VERTEX_POINT('',#9883);
#2722=VERTEX_POINT('',#9885);
#2723=VERTEX_POINT('',#9887);
#2724=VERTEX_POINT('',#9889);
#2725=VERTEX_POINT('',#9891);
#2726=VERTEX_POINT('',#9893);
#2727=VERTEX_POINT('',#9895);
#2728=VERTEX_POINT('',#9898);
#2729=VERTEX_POINT('',#9901);
#2730=VERTEX_POINT('',#9903);
#2731=VERTEX_POINT('',#9908);
#2732=VERTEX_POINT('',#9934);
#2733=VERTEX_POINT('',#9957);
#2734=VERTEX_POINT('',#9961);
#2735=VERTEX_POINT('',#9963);
#2736=VERTEX_POINT('',#9965);
#2737=VERTEX_POINT('',#9967);
#2738=VERTEX_POINT('',#9971);
#2739=VERTEX_POINT('',#9974);
#2740=VERTEX_POINT('',#9975);
#2741=VERTEX_POINT('',#9978);
#2742=VERTEX_POINT('',#9985);
#2743=VERTEX_POINT('',#9987);
#2744=VERTEX_POINT('',#9989);
#2745=VERTEX_POINT('',#9991);
#2746=VERTEX_POINT('',#9993);
#2747=VERTEX_POINT('',#10001);
#2748=VERTEX_POINT('',#10004);
#2749=VERTEX_POINT('',#10005);
#2750=VERTEX_POINT('',#10030);
#2751=VERTEX_POINT('',#10035);
#2752=VERTEX_POINT('',#10059);
#2753=VERTEX_POINT('',#10062);
#2754=VERTEX_POINT('',#10066);
#2755=VERTEX_POINT('',#10067);
#2756=VERTEX_POINT('',#10069);
#2757=VERTEX_POINT('',#10071);
#2758=VERTEX_POINT('',#10073);
#2759=VERTEX_POINT('',#10085);
#2760=VERTEX_POINT('',#10096);
#2761=VERTEX_POINT('',#10098);
#2762=VERTEX_POINT('',#10104);
#2763=VERTEX_POINT('',#10106);
#2764=VERTEX_POINT('',#10108);
#2765=VERTEX_POINT('',#10112);
#2766=VERTEX_POINT('',#10113);
#2767=VERTEX_POINT('',#10118);
#2768=VERTEX_POINT('',#10119);
#2769=VERTEX_POINT('',#10122);
#2770=VERTEX_POINT('',#10125);
#2771=VERTEX_POINT('',#10127);
#2772=VERTEX_POINT('',#10129);
#2773=VERTEX_POINT('',#10131);
#2774=VERTEX_POINT('',#10133);
#2775=VERTEX_POINT('',#10136);
#2776=VERTEX_POINT('',#10257);
#2777=VERTEX_POINT('',#10261);
#2778=VERTEX_POINT('',#10263);
#2779=VERTEX_POINT('',#10267);
#2780=VERTEX_POINT('',#10269);
#2781=VERTEX_POINT('',#10271);
#2782=VERTEX_POINT('',#10276);
#2783=VERTEX_POINT('',#10280);
#2784=VERTEX_POINT('',#10282);
#2785=VERTEX_POINT('',#10285);
#2786=VERTEX_POINT('',#10287);
#2787=VERTEX_POINT('',#10290);
#2788=VERTEX_POINT('',#10296);
#2789=VERTEX_POINT('',#10298);
#2790=VERTEX_POINT('',#10304);
#2791=VERTEX_POINT('',#10310);
#2792=VERTEX_POINT('',#10323);
#2793=VERTEX_POINT('',#10327);
#2794=VERTEX_POINT('',#10349);
#2795=VERTEX_POINT('',#10351);
#2796=VERTEX_POINT('',#10355);
#2797=VERTEX_POINT('',#10358);
#2798=VERTEX_POINT('',#10360);
#2799=VERTEX_POINT('',#10364);
#2800=VERTEX_POINT('',#10368);
#2801=VERTEX_POINT('',#10369);
#2802=VERTEX_POINT('',#10371);
#2803=VERTEX_POINT('',#10373);
#2804=VERTEX_POINT('',#10375);
#2805=VERTEX_POINT('',#10377);
#2806=VERTEX_POINT('',#10380);
#2807=VERTEX_POINT('',#10383);
#2808=VERTEX_POINT('',#10385);
#2809=VERTEX_POINT('',#10389);
#2810=VERTEX_POINT('',#10393);
#2811=VERTEX_POINT('',#10397);
#2812=VERTEX_POINT('',#10401);
#2813=VERTEX_POINT('',#10407);
#2814=VERTEX_POINT('',#10410);
#2815=VERTEX_POINT('',#10414);
#2816=VERTEX_POINT('',#10418);
#2817=VERTEX_POINT('',#10421);
#2818=VERTEX_POINT('',#10426);
#2819=VERTEX_POINT('',#10428);
#2820=VERTEX_POINT('',#10432);
#2821=VERTEX_POINT('',#10435);
#2822=VERTEX_POINT('',#10437);
#2823=VERTEX_POINT('',#10441);
#2824=VERTEX_POINT('',#10450);
#2825=VERTEX_POINT('',#10452);
#2826=VERTEX_POINT('',#10455);
#2827=VERTEX_POINT('',#10458);
#2828=VERTEX_POINT('',#10459);
#2829=VERTEX_POINT('',#10497);
#2830=VERTEX_POINT('',#10533);
#2831=VERTEX_POINT('',#10535);
#2832=VERTEX_POINT('',#10537);
#2833=VERTEX_POINT('',#10539);
#2834=VERTEX_POINT('',#10541);
#2835=VERTEX_POINT('',#10543);
#2836=VERTEX_POINT('',#10545);
#2837=VERTEX_POINT('',#10547);
#2838=VERTEX_POINT('',#10549);
#2839=VERTEX_POINT('',#10552);
#2840=VERTEX_POINT('',#10556);
#2841=VERTEX_POINT('',#10559);
#2842=VERTEX_POINT('',#10563);
#2843=VERTEX_POINT('',#10566);
#2844=VERTEX_POINT('',#10570);
#2845=VERTEX_POINT('',#10572);
#2846=VERTEX_POINT('',#10574);
#2847=VERTEX_POINT('',#10576);
#2848=VERTEX_POINT('',#10578);
#2849=VERTEX_POINT('',#10580);
#2850=VERTEX_POINT('',#10582);
#2851=VERTEX_POINT('',#10584);
#2852=VERTEX_POINT('',#10586);
#2853=VERTEX_POINT('',#10589);
#2854=VERTEX_POINT('',#10593);
#2855=VERTEX_POINT('',#10597);
#2856=VERTEX_POINT('',#10632);
#2857=VERTEX_POINT('',#10633);
#2858=VERTEX_POINT('',#10694);
#2859=VERTEX_POINT('',#10696);
#2860=VERTEX_POINT('',#10698);
#2861=VERTEX_POINT('',#10709);
#2862=VERTEX_POINT('',#10711);
#2863=VERTEX_POINT('',#10722);
#2864=VERTEX_POINT('',#10746);
#2865=VERTEX_POINT('',#10748);
#2866=VERTEX_POINT('',#10750);
#2867=VERTEX_POINT('',#10772);
#2868=VERTEX_POINT('',#10773);
#2869=VERTEX_POINT('',#10775);
#2870=VERTEX_POINT('',#10777);
#2871=VERTEX_POINT('',#10780);
#2872=VERTEX_POINT('',#10782);
#2873=VERTEX_POINT('',#10785);
#2874=VERTEX_POINT('',#10789);
#2875=VERTEX_POINT('',#10790);
#2876=VERTEX_POINT('',#10792);
#2877=VERTEX_POINT('',#10794);
#2878=VERTEX_POINT('',#10798);
#2879=VERTEX_POINT('',#10809);
#2880=VERTEX_POINT('',#10821);
#2881=VERTEX_POINT('',#10822);
#2882=VERTEX_POINT('',#10825);
#2883=VERTEX_POINT('',#10835);
#2884=VERTEX_POINT('',#10851);
#2885=VERTEX_POINT('',#10853);
#2886=VERTEX_POINT('',#10892);
#2887=VERTEX_POINT('',#10893);
#2888=VERTEX_POINT('',#10935);
#2889=VERTEX_POINT('',#10940);
#2890=VERTEX_POINT('',#10942);
#2891=VERTEX_POINT('',#10946);
#2892=VERTEX_POINT('',#10950);
#2893=VERTEX_POINT('',#10953);
#2894=VERTEX_POINT('',#10957);
#2895=VERTEX_POINT('',#10960);
#2896=VERTEX_POINT('',#10964);
#2897=VERTEX_POINT('',#10967);
#2898=VERTEX_POINT('',#10969);
#2899=VERTEX_POINT('',#10971);
#2900=VERTEX_POINT('',#10973);
#2901=VERTEX_POINT('',#10975);
#2902=VERTEX_POINT('',#10977);
#2903=VERTEX_POINT('',#10979);
#2904=VERTEX_POINT('',#10981);
#2905=VERTEX_POINT('',#10983);
#2906=VERTEX_POINT('',#10996);
#2907=VERTEX_POINT('',#10998);
#2908=VERTEX_POINT('',#11002);
#2909=VERTEX_POINT('',#11006);
#2910=VERTEX_POINT('',#11009);
#2911=VERTEX_POINT('',#11011);
#2912=VERTEX_POINT('',#11013);
#2913=VERTEX_POINT('',#11032);
#2914=VERTEX_POINT('',#11034);
#2915=VERTEX_POINT('',#11092);
#2916=VERTEX_POINT('',#11093);
#2917=VERTEX_POINT('',#11131);
#2918=VERTEX_POINT('',#11167);
#2919=VERTEX_POINT('',#11171);
#2920=VERTEX_POINT('',#11176);
#2921=VERTEX_POINT('',#11180);
#2922=VERTEX_POINT('',#11195);
#2923=VERTEX_POINT('',#11196);
#2924=VERTEX_POINT('',#11198);
#2925=VERTEX_POINT('',#11200);
#2926=VERTEX_POINT('',#11204);
#2927=VERTEX_POINT('',#11206);
#2928=VERTEX_POINT('',#11210);
#2929=VERTEX_POINT('',#11212);
#2930=VERTEX_POINT('',#11214);
#2931=VERTEX_POINT('',#11217);
#2932=VERTEX_POINT('',#11219);
#2933=VERTEX_POINT('',#11222);
#2934=VERTEX_POINT('',#11223);
#2935=VERTEX_POINT('',#11262);
#2936=VERTEX_POINT('',#11264);
#2937=VERTEX_POINT('',#11267);
#2938=VERTEX_POINT('',#11268);
#2939=VERTEX_POINT('',#11306);
#2940=VERTEX_POINT('',#11308);
#2941=VERTEX_POINT('',#11310);
#2942=VERTEX_POINT('',#11312);
#2943=VERTEX_POINT('',#11315);
#2944=VERTEX_POINT('',#11317);
#2945=VERTEX_POINT('',#11321);
#2946=VERTEX_POINT('',#11325);
#2947=VERTEX_POINT('',#11327);
#2948=VERTEX_POINT('',#11329);
#2949=VERTEX_POINT('',#11331);
#2950=VERTEX_POINT('',#11340);
#2951=VERTEX_POINT('',#11342);
#2952=VERTEX_POINT('',#11346);
#2953=VERTEX_POINT('',#11348);
#2954=VERTEX_POINT('',#11351);
#2955=VERTEX_POINT('',#11354);
#2956=VERTEX_POINT('',#11392);
#2957=VERTEX_POINT('',#11393);
#2958=VERTEX_POINT('',#11414);
#2959=VERTEX_POINT('',#11419);
#2960=VERTEX_POINT('',#11421);
#2961=VERTEX_POINT('',#11425);
#2962=VERTEX_POINT('',#11428);
#2963=VERTEX_POINT('',#11430);
#2964=VERTEX_POINT('',#11434);
#2965=VERTEX_POINT('',#11437);
#2966=VERTEX_POINT('',#11439);
#2967=VERTEX_POINT('',#11443);
#2968=VERTEX_POINT('',#11446);
#2969=VERTEX_POINT('',#11448);
#2970=VERTEX_POINT('',#11452);
#2971=VERTEX_POINT('',#11455);
#2972=VERTEX_POINT('',#11457);
#2973=VERTEX_POINT('',#11461);
#2974=VERTEX_POINT('',#11465);
#2975=VERTEX_POINT('',#11467);
#2976=VERTEX_POINT('',#11469);
#2977=VERTEX_POINT('',#11471);
#2978=VERTEX_POINT('',#11473);
#2979=VERTEX_POINT('',#11476);
#2980=VERTEX_POINT('',#11480);
#2981=VERTEX_POINT('',#11483);
#2982=VERTEX_POINT('',#11487);
#2983=VERTEX_POINT('',#11490);
#2984=VERTEX_POINT('',#11492);
#2985=VERTEX_POINT('',#11496);
#2986=VERTEX_POINT('',#11500);
#2987=VERTEX_POINT('',#11502);
#2988=VERTEX_POINT('',#11504);
#2989=VERTEX_POINT('',#11506);
#2990=VERTEX_POINT('',#11515);
#2991=VERTEX_POINT('',#11517);
#2992=VERTEX_POINT('',#11524);
#2993=VERTEX_POINT('',#11525);
#2994=VERTEX_POINT('',#11920);
#2995=VERTEX_POINT('',#12474);
#2996=VERTEX_POINT('',#13580);
#2997=VERTEX_POINT('',#14098);
#2998=VERTEX_POINT('',#15345);
#2999=VERTEX_POINT('',#15899);
#3000=VERTEX_POINT('',#16709);
#3001=VERTEX_POINT('',#16710);
#3002=VERTEX_POINT('',#16712);
#3003=VERTEX_POINT('',#16714);
#3004=VERTEX_POINT('',#16716);
#3005=VERTEX_POINT('',#16718);
#3006=VERTEX_POINT('',#16721);
#3007=VERTEX_POINT('',#16724);
#3008=VERTEX_POINT('',#16728);
#3009=VERTEX_POINT('',#16729);
#3010=VERTEX_POINT('',#16731);
#3011=VERTEX_POINT('',#16733);
#3012=VERTEX_POINT('',#16735);
#3013=VERTEX_POINT('',#16737);
#3014=VERTEX_POINT('',#16753);
#3015=VERTEX_POINT('',#16755);
#3016=VERTEX_POINT('',#16759);
#3017=VERTEX_POINT('',#16764);
#3018=VERTEX_POINT('',#16765);
#3019=VERTEX_POINT('',#16767);
#3020=VERTEX_POINT('',#16769);
#3021=VERTEX_POINT('',#16771);
#3022=VERTEX_POINT('',#16773);
#3023=VERTEX_POINT('',#16775);
#3024=VERTEX_POINT('',#16777);
#3025=VERTEX_POINT('',#16781);
#3026=VERTEX_POINT('',#16782);
#3027=VERTEX_POINT('',#16787);
#3028=VERTEX_POINT('',#16790);
#3029=VERTEX_POINT('',#16792);
#3030=VERTEX_POINT('',#16794);
#3031=VERTEX_POINT('',#16796);
#3032=VERTEX_POINT('',#16800);
#3033=VERTEX_POINT('',#16801);
#3034=VERTEX_POINT('',#16803);
#3035=VERTEX_POINT('',#16805);
#3036=VERTEX_POINT('',#16807);
#3037=VERTEX_POINT('',#16809);
#3038=VERTEX_POINT('',#16813);
#3039=VERTEX_POINT('',#16817);
#3040=VERTEX_POINT('',#16820);
#3041=VERTEX_POINT('',#16822);
#3042=VERTEX_POINT('',#16841);
#3043=VERTEX_POINT('',#16844);
#3044=VERTEX_POINT('',#16863);
#3045=VERTEX_POINT('',#16865);
#3046=VERTEX_POINT('',#16869);
#3047=VERTEX_POINT('',#16873);
#3048=VERTEX_POINT('',#16875);
#3049=VERTEX_POINT('',#16878);
#3050=VERTEX_POINT('',#16883);
#3051=VERTEX_POINT('',#16888);
#3052=VERTEX_POINT('',#16890);
#3053=VERTEX_POINT('',#16894);
#3054=VERTEX_POINT('',#16897);
#3055=VERTEX_POINT('',#16899);
#3056=VERTEX_POINT('',#16903);
#3057=VERTEX_POINT('',#16907);
#3058=VERTEX_POINT('',#16909);
#3059=VERTEX_POINT('',#16912);
#3060=VERTEX_POINT('',#16916);
#3061=VERTEX_POINT('',#16919);
#3062=VERTEX_POINT('',#16923);
#3063=VERTEX_POINT('',#16926);
#3064=VERTEX_POINT('',#16930);
#3065=VERTEX_POINT('',#16935);
#3066=VERTEX_POINT('',#16937);
#3067=VERTEX_POINT('',#16941);
#3068=VERTEX_POINT('',#16953);
#3069=VERTEX_POINT('',#16954);
#3070=VERTEX_POINT('',#16956);
#3071=VERTEX_POINT('',#16958);
#3072=VERTEX_POINT('',#16960);
#3073=VERTEX_POINT('',#16962);
#3074=VERTEX_POINT('',#16964);
#3075=VERTEX_POINT('',#16966);
#3076=VERTEX_POINT('',#16969);
#3077=VERTEX_POINT('',#16971);
#3078=VERTEX_POINT('',#16974);
#3079=VERTEX_POINT('',#16978);
#3080=VERTEX_POINT('',#16979);
#3081=VERTEX_POINT('',#16981);
#3082=VERTEX_POINT('',#16983);
#3083=VERTEX_POINT('',#16985);
#3084=VERTEX_POINT('',#16987);
#3085=VERTEX_POINT('',#16989);
#3086=VERTEX_POINT('',#16991);
#3087=VERTEX_POINT('',#16994);
#3088=VERTEX_POINT('',#16997);
#3089=VERTEX_POINT('',#16998);
#3090=VERTEX_POINT('',#17003);
#3091=VERTEX_POINT('',#17004);
#3092=VERTEX_POINT('',#17006);
#3093=VERTEX_POINT('',#17008);
#3094=VERTEX_POINT('',#17010);
#3095=VERTEX_POINT('',#17012);
#3096=VERTEX_POINT('',#17014);
#3097=VERTEX_POINT('',#17016);
#3098=VERTEX_POINT('',#17019);
#3099=VERTEX_POINT('',#17021);
#3100=VERTEX_POINT('',#17023);
#3101=VERTEX_POINT('',#17025);
#3102=VERTEX_POINT('',#17027);
#3103=VERTEX_POINT('',#17029);
#3104=EDGE_CURVE('',#2582,#2583,#1860,.T.);
#3105=EDGE_CURVE('',#2584,#2583,#1861,.T.);
#3106=EDGE_CURVE('',#2585,#2584,#1862,.T.);
#3107=EDGE_CURVE('',#2582,#2585,#1863,.T.);
#3108=EDGE_CURVE('',#2586,#2582,#1864,.T.);
#3109=EDGE_CURVE('',#2586,#2587,#1865,.T.);
#3110=EDGE_CURVE('',#2587,#2583,#1866,.T.);
#3111=EDGE_CURVE('',#2588,#2589,#1867,.T.);
#3112=EDGE_CURVE('',#2589,#2583,#1868,.T.);
#3113=EDGE_CURVE('',#2588,#2587,#1869,.T.);
#3114=EDGE_CURVE('',#2590,#2591,#1870,.T.);
#3115=EDGE_CURVE('',#2589,#2591,#1871,.T.);
#3116=EDGE_CURVE('',#2588,#2592,#1872,.T.);
#3117=EDGE_CURVE('',#2593,#2592,#1873,.T.);
#3118=EDGE_CURVE('',#2593,#2590,#1874,.T.);
#3119=EDGE_CURVE('',#2594,#2594,#636,.T.);
#3120=EDGE_CURVE('',#2595,#2595,#637,.T.);
#3121=EDGE_CURVE('',#2590,#2596,#1875,.T.);
#3122=EDGE_CURVE('',#2596,#2597,#1876,.T.);
#3123=EDGE_CURVE('',#2597,#2591,#1877,.T.);
#3124=EDGE_CURVE('',#2584,#2597,#1878,.T.);
#3125=EDGE_CURVE('',#2585,#2596,#1879,.T.);
#3126=EDGE_CURVE('',#2598,#2598,#638,.T.);
#3127=EDGE_CURVE('',#2599,#2599,#639,.T.);
#3128=EDGE_CURVE('',#2600,#2600,#640,.T.);
#3129=EDGE_CURVE('',#2601,#2601,#641,.T.);
#3130=EDGE_CURVE('',#2593,#2582,#1880,.T.);
#3131=EDGE_CURVE('',#2592,#2586,#1881,.T.);
#3132=EDGE_CURVE('',#2602,#2602,#642,.T.);
#3133=EDGE_CURVE('',#2603,#2603,#643,.T.);
#3134=EDGE_CURVE('',#2604,#2604,#644,.T.);
#3135=EDGE_CURVE('',#2605,#2605,#645,.T.);
#3136=EDGE_CURVE('',#2598,#2602,#1882,.T.);
#3137=EDGE_CURVE('',#2599,#2603,#1883,.T.);
#3138=EDGE_CURVE('',#2600,#2604,#1884,.T.);
#3139=EDGE_CURVE('',#2601,#2605,#1885,.T.);
#3140=EDGE_CURVE('',#2606,#2606,#646,.T.);
#3141=EDGE_CURVE('',#2606,#2594,#1886,.T.);
#3142=EDGE_CURVE('',#2607,#2607,#647,.T.);
#3143=EDGE_CURVE('',#2607,#2595,#1887,.T.);
#3144=EDGE_CURVE('',#2608,#2609,#648,.T.);
#3145=EDGE_CURVE('',#2610,#2608,#1888,.T.);
#3146=EDGE_CURVE('',#2611,#2610,#649,.T.);
#3147=EDGE_CURVE('',#2612,#2611,#1889,.T.);
#3148=EDGE_CURVE('',#2613,#2612,#650,.T.);
#3149=EDGE_CURVE('',#2614,#2613,#1890,.T.);
#3150=EDGE_CURVE('',#2615,#2614,#651,.T.);
#3151=EDGE_CURVE('',#2609,#2615,#1891,.T.);
#3152=EDGE_CURVE('',#2616,#2616,#652,.T.);
#3153=EDGE_CURVE('',#2617,#2617,#653,.T.);
#3154=EDGE_CURVE('',#2618,#2618,#654,.T.);
#3155=EDGE_CURVE('',#2619,#2619,#655,.T.);
#3156=EDGE_CURVE('',#2620,#2620,#656,.T.);
#3157=EDGE_CURVE('',#2621,#2621,#657,.T.);
#3158=EDGE_CURVE('',#2621,#2622,#1892,.T.);
#3159=EDGE_CURVE('',#2622,#2622,#658,.T.);
#3160=EDGE_CURVE('',#2623,#2624,#659,.T.);
#3161=EDGE_CURVE('',#2624,#2625,#1893,.T.);
#3162=EDGE_CURVE('',#2625,#2626,#660,.T.);
#3163=EDGE_CURVE('',#2626,#2627,#1894,.T.);
#3164=EDGE_CURVE('',#2627,#2628,#661,.T.);
#3165=EDGE_CURVE('',#2628,#2629,#1895,.T.);
#3166=EDGE_CURVE('',#2629,#2630,#662,.T.);
#3167=EDGE_CURVE('',#2630,#2623,#1896,.T.);
#3168=EDGE_CURVE('',#2631,#2631,#663,.T.);
#3169=EDGE_CURVE('',#2632,#2632,#664,.T.);
#3170=EDGE_CURVE('',#2633,#2633,#665,.T.);
#3171=EDGE_CURVE('',#2634,#2634,#666,.T.);
#3172=EDGE_CURVE('',#2635,#2635,#667,.T.);
#3173=EDGE_CURVE('',#2616,#2631,#1897,.T.);
#3174=EDGE_CURVE('',#2617,#2632,#1898,.T.);
#3175=EDGE_CURVE('',#2618,#2633,#1899,.T.);
#3176=EDGE_CURVE('',#2619,#2634,#1900,.T.);
#3177=EDGE_CURVE('',#2620,#2635,#1901,.T.);
#3178=EDGE_CURVE('',#2623,#2636,#1902,.T.);
#3179=EDGE_CURVE('',#2636,#2637,#668,.T.);
#3180=EDGE_CURVE('',#2624,#2637,#1903,.T.);
#3181=EDGE_CURVE('',#2637,#2638,#1904,.T.);
#3182=EDGE_CURVE('',#2625,#2638,#1905,.T.);
#3183=EDGE_CURVE('',#2638,#2639,#669,.T.);
#3184=EDGE_CURVE('',#2626,#2639,#1906,.T.);
#3185=EDGE_CURVE('',#2639,#2640,#1907,.T.);
#3186=EDGE_CURVE('',#2627,#2640,#1908,.T.);
#3187=EDGE_CURVE('',#2640,#2641,#670,.T.);
#3188=EDGE_CURVE('',#2628,#2641,#1909,.T.);
#3189=EDGE_CURVE('',#2641,#2642,#1910,.T.);
#3190=EDGE_CURVE('',#2629,#2642,#1911,.T.);
#3191=EDGE_CURVE('',#2642,#2643,#671,.T.);
#3192=EDGE_CURVE('',#2630,#2643,#1912,.T.);
#3193=EDGE_CURVE('',#2643,#2636,#1913,.T.);
#3194=EDGE_CURVE('',#2612,#2643,#1914,.T.);
#3195=EDGE_CURVE('',#2611,#2636,#1915,.T.);
#3196=EDGE_CURVE('',#2610,#2637,#1916,.T.);
#3197=EDGE_CURVE('',#2608,#2638,#1917,.T.);
#3198=EDGE_CURVE('',#2609,#2639,#1918,.T.);
#3199=EDGE_CURVE('',#2615,#2640,#1919,.T.);
#3200=EDGE_CURVE('',#2614,#2641,#1920,.T.);
#3201=EDGE_CURVE('',#2613,#2642,#1921,.T.);
#3202=EDGE_CURVE('',#2644,#2644,#672,.T.);
#3203=EDGE_CURVE('',#2644,#2645,#1922,.T.);
#3204=EDGE_CURVE('',#2645,#2645,#673,.T.);
#3205=EDGE_CURVE('',#2646,#2646,#674,.T.);
#3206=EDGE_CURVE('',#2647,#2647,#675,.T.);
#3207=EDGE_CURVE('',#2647,#2648,#1923,.T.);
#3208=EDGE_CURVE('',#2648,#2648,#676,.T.);
#3209=EDGE_CURVE('',#2649,#2649,#677,.T.);
#3210=EDGE_CURVE('',#2650,#2651,#1924,.T.);
#3211=EDGE_CURVE('',#2651,#2652,#1925,.T.);
#3212=EDGE_CURVE('',#2652,#2653,#1926,.T.);
#3213=EDGE_CURVE('',#2653,#2654,#146,.T.);
#3214=EDGE_CURVE('',#2654,#2655,#1927,.T.);
#3215=EDGE_CURVE('',#2655,#2650,#1928,.T.);
#3216=EDGE_CURVE('',#2656,#2656,#678,.T.);
#3217=EDGE_CURVE('',#2656,#2657,#1929,.T.);
#3218=EDGE_CURVE('',#2658,#2657,#679,.T.);
#3219=EDGE_CURVE('',#2657,#2658,#680,.T.);
#3220=EDGE_CURVE('',#2658,#2659,#681,.T.);
#3221=EDGE_CURVE('',#2659,#2659,#682,.T.);
#3222=EDGE_CURVE('',#2660,#2660,#683,.T.);
#3223=EDGE_CURVE('',#2660,#2661,#1930,.T.);
#3224=EDGE_CURVE('',#2661,#2661,#684,.T.);
#3225=EDGE_CURVE('',#2662,#2663,#147,.T.);
#3226=EDGE_CURVE('',#2663,#2662,#148,.T.);
#3227=EDGE_CURVE('',#2664,#2664,#685,.T.);
#3228=EDGE_CURVE('',#2664,#2665,#686,.T.);
#3229=EDGE_CURVE('',#2665,#2666,#687,.T.);
#3230=EDGE_CURVE('',#2666,#2665,#688,.T.);
#3231=EDGE_CURVE('',#2666,#2667,#1931,.T.);
#3232=EDGE_CURVE('',#2667,#2667,#689,.T.);
#3233=EDGE_CURVE('',#2668,#2669,#1932,.T.);
#3234=EDGE_CURVE('',#2669,#2670,#1933,.T.);
#3235=EDGE_CURVE('',#2670,#2671,#1934,.T.);
#3236=EDGE_CURVE('',#2671,#2672,#1935,.T.);
#3237=EDGE_CURVE('',#2672,#2673,#149,.T.);
#3238=EDGE_CURVE('',#2673,#2668,#1936,.T.);
#3239=EDGE_CURVE('',#2674,#2675,#1937,.T.);
#3240=EDGE_CURVE('',#2669,#2675,#690,.T.);
#3241=EDGE_CURVE('',#2674,#2668,#691,.T.);
#3242=EDGE_CURVE('',#2674,#2676,#1938,.T.);
#3243=EDGE_CURVE('',#2677,#2676,#1939,.T.);
#3244=EDGE_CURVE('',#2675,#2677,#1940,.T.);
#3245=EDGE_CURVE('',#2678,#2674,#692,.T.);
#3246=EDGE_CURVE('',#2678,#2679,#1941,.T.);
#3247=EDGE_CURVE('',#2676,#2679,#693,.T.);
#3248=EDGE_CURVE('',#2679,#2652,#694,.T.);
#3249=EDGE_CURVE('',#2652,#2676,#695,.T.);
#3250=EDGE_CURVE('',#2679,#2680,#1942,.T.);
#3251=EDGE_CURVE('',#2653,#2680,#696,.T.);
#3252=EDGE_CURVE('',#2680,#2681,#150,.T.);
#3253=EDGE_CURVE('',#2654,#2681,#697,.T.);
#3254=EDGE_CURVE('',#2681,#2682,#1943,.T.);
#3255=EDGE_CURVE('',#2655,#2682,#698,.T.);
#3256=EDGE_CURVE('',#2683,#2678,#1944,.T.);
#3257=EDGE_CURVE('',#2684,#2683,#699,.T.);
#3258=EDGE_CURVE('',#2680,#2684,#700,.T.);
#3259=EDGE_CURVE('',#2685,#2681,#701,.T.);
#3260=EDGE_CURVE('',#2686,#2685,#1945,.T.);
#3261=EDGE_CURVE('',#2686,#2682,#1946,.T.);
#3262=EDGE_CURVE('',#2684,#2687,#702,.T.);
#3263=EDGE_CURVE('',#2688,#2687,#703,.T.);
#3264=EDGE_CURVE('',#2687,#2688,#704,.T.);
#3265=EDGE_CURVE('',#2685,#2683,#151,.T.);
#3266=EDGE_CURVE('',#2672,#2685,#705,.T.);
#3267=EDGE_CURVE('',#2673,#2683,#706,.T.);
#3268=EDGE_CURVE('',#2668,#2678,#707,.T.);
#3269=EDGE_CURVE('',#2686,#2671,#708,.T.);
#3270=EDGE_CURVE('',#2671,#2689,#709,.T.);
#3271=EDGE_CURVE('',#2689,#2686,#710,.T.);
#3272=EDGE_CURVE('',#2689,#2690,#1947,.T.);
#3273=EDGE_CURVE('',#2682,#2690,#711,.T.);
#3274=EDGE_CURVE('',#2690,#2655,#712,.T.);
#3275=EDGE_CURVE('',#2690,#2691,#1948,.T.);
#3276=EDGE_CURVE('',#2650,#2691,#713,.T.);
#3277=EDGE_CURVE('',#2692,#2689,#1949,.T.);
#3278=EDGE_CURVE('',#2692,#2691,#1950,.T.);
#3279=EDGE_CURVE('',#2693,#2692,#714,.T.);
#3280=EDGE_CURVE('',#2693,#2694,#1951,.T.);
#3281=EDGE_CURVE('',#2691,#2694,#715,.T.);
#3282=EDGE_CURVE('',#2694,#2650,#716,.T.);
#3283=EDGE_CURVE('',#2694,#2695,#1952,.T.);
#3284=EDGE_CURVE('',#2651,#2695,#717,.T.);
#3285=EDGE_CURVE('',#2677,#2651,#718,.T.);
#3286=EDGE_CURVE('',#2695,#2677,#719,.T.);
#3287=EDGE_CURVE('',#2696,#2695,#1953,.T.);
#3288=EDGE_CURVE('',#2675,#2696,#720,.T.);
#3289=EDGE_CURVE('',#2696,#2693,#1954,.T.);
#3290=EDGE_CURVE('',#2697,#2697,#721,.T.);
#3291=EDGE_CURVE('',#2670,#2693,#722,.T.);
#3292=EDGE_CURVE('',#2696,#2669,#723,.T.);
#3293=EDGE_CURVE('',#2692,#2670,#724,.T.);
#3294=EDGE_CURVE('',#2698,#2698,#725,.T.);
#3295=EDGE_CURVE('',#2698,#2697,#1955,.T.);
#3296=EDGE_CURVE('',#2699,#2699,#726,.T.);
#3297=EDGE_CURVE('',#2700,#2700,#727,.T.);
#3298=EDGE_CURVE('',#2700,#2699,#1956,.T.);
#3299=EDGE_CURVE('',#2663,#2700,#1957,.T.);
#3300=EDGE_CURVE('',#2701,#2702,#728,.T.);
#3301=EDGE_CURVE('',#2702,#2688,#1958,.T.);
#3302=EDGE_CURVE('',#2702,#2701,#729,.T.);
#3303=EDGE_CURVE('',#2703,#2704,#730,.T.);
#3304=EDGE_CURVE('',#2704,#2703,#731,.T.);
#3305=EDGE_CURVE('',#2703,#2705,#1959,.T.);
#3306=EDGE_CURVE('',#2706,#2705,#732,.T.);
#3307=EDGE_CURVE('',#2705,#2706,#733,.T.);
#3308=EDGE_CURVE('',#2701,#2706,#734,.T.);
#3309=EDGE_CURVE('',#2704,#2707,#735,.T.);
#3310=EDGE_CURVE('',#2708,#2707,#152,.T.);
#3311=EDGE_CURVE('',#2708,#2709,#736,.T.);
#3312=EDGE_CURVE('',#2709,#2710,#153,.T.);
#3313=EDGE_CURVE('',#2710,#2711,#154,.T.);
#3314=EDGE_CURVE('',#2711,#2712,#737,.T.);
#3315=EDGE_CURVE('',#2712,#2713,#155,.F.);
#3316=EDGE_CURVE('',#2713,#2714,#738,.T.);
#3317=EDGE_CURVE('',#2715,#2714,#156,.T.);
#3318=EDGE_CURVE('',#2715,#2716,#739,.T.);
#3319=EDGE_CURVE('',#2707,#2716,#157,.T.);
#3320=EDGE_CURVE('',#2717,#2718,#158,.T.);
#3321=EDGE_CURVE('',#2717,#2715,#740,.T.);
#3322=EDGE_CURVE('',#2718,#2714,#741,.T.);
#3323=EDGE_CURVE('',#2719,#2717,#1960,.T.);
#3324=EDGE_CURVE('',#2718,#2720,#1961,.T.);
#3325=EDGE_CURVE('',#2721,#2720,#1962,.T.);
#3326=EDGE_CURVE('',#2721,#2722,#1963,.T.);
#3327=EDGE_CURVE('',#2722,#2723,#742,.T.);
#3328=EDGE_CURVE('',#2724,#2723,#1964,.T.);
#3329=EDGE_CURVE('',#2724,#2725,#1965,.T.);
#3330=EDGE_CURVE('',#2725,#2726,#1966,.T.);
#3331=EDGE_CURVE('',#2727,#2726,#1967,.T.);
#3332=EDGE_CURVE('',#2719,#2727,#1968,.T.);
#3333=EDGE_CURVE('',#2728,#2728,#743,.T.);
#3334=EDGE_CURVE('',#2728,#2729,#1969,.T.);
#3335=EDGE_CURVE('',#2730,#2729,#159,.F.);
#3336=EDGE_CURVE('',#2731,#2730,#160,.F.);
#3337=EDGE_CURVE('',#2731,#2732,#1970,.T.);
#3338=EDGE_CURVE('',#2732,#2732,#744,.T.);
#3339=EDGE_CURVE('',#2729,#2731,#161,.F.);
#3340=EDGE_CURVE('',#2730,#2733,#1971,.T.);
#3341=EDGE_CURVE('',#2733,#2733,#745,.T.);
#3342=EDGE_CURVE('',#2734,#2719,#746,.T.);
#3343=EDGE_CURVE('',#2727,#2735,#1972,.T.);
#3344=EDGE_CURVE('',#2735,#2736,#1973,.T.);
#3345=EDGE_CURVE('',#2736,#2737,#747,.T.);
#3346=EDGE_CURVE('',#2737,#2708,#1974,.T.);
#3347=EDGE_CURVE('',#2716,#2734,#1975,.T.);
#3348=EDGE_CURVE('',#2738,#2738,#748,.T.);
#3349=EDGE_CURVE('',#2739,#2740,#1976,.T.);
#3350=EDGE_CURVE('',#2724,#2740,#1977,.T.);
#3351=EDGE_CURVE('',#2741,#2723,#162,.T.);
#3352=EDGE_CURVE('',#2741,#2742,#1978,.T.);
#3353=EDGE_CURVE('',#2742,#2743,#1979,.T.);
#3354=EDGE_CURVE('',#2743,#2744,#1980,.T.);
#3355=EDGE_CURVE('',#2744,#2745,#1981,.T.);
#3356=EDGE_CURVE('',#2745,#2746,#1982,.T.);
#3357=EDGE_CURVE('',#2739,#2746,#163,.T.);
#3358=EDGE_CURVE('',#2747,#2747,#749,.T.);
#3359=EDGE_CURVE('',#2748,#2749,#164,.T.);
#3360=EDGE_CURVE('',#2749,#2747,#1983,.T.);
#3361=EDGE_CURVE('',#2749,#2750,#165,.T.);
#3362=EDGE_CURVE('',#2750,#2751,#166,.T.);
#3363=EDGE_CURVE('',#2751,#2748,#167,.T.);
#3364=EDGE_CURVE('',#2752,#2752,#750,.T.);
#3365=EDGE_CURVE('',#2752,#2750,#1984,.T.);
#3366=EDGE_CURVE('',#2751,#2753,#1985,.T.);
#3367=EDGE_CURVE('',#2753,#2753,#751,.T.);
#3368=EDGE_CURVE('',#2754,#2755,#1986,.T.);
#3369=EDGE_CURVE('',#2756,#2754,#1987,.T.);
#3370=EDGE_CURVE('',#2757,#2756,#1988,.T.);
#3371=EDGE_CURVE('',#2758,#2757,#168,.T.);
#3372=EDGE_CURVE('',#2759,#2758,#169,.T.);
#3373=EDGE_CURVE('',#2736,#2759,#1989,.T.);
#3374=EDGE_CURVE('',#2735,#2760,#1990,.T.);
#3375=EDGE_CURVE('',#2761,#2760,#1991,.T.);
#3376=EDGE_CURVE('',#2740,#2761,#1992,.T.);
#3377=EDGE_CURVE('',#2739,#2755,#752,.T.);
#3378=EDGE_CURVE('',#2762,#2755,#753,.T.);
#3379=EDGE_CURVE('',#2763,#2762,#1993,.T.);
#3380=EDGE_CURVE('',#2764,#2763,#1994,.T.);
#3381=EDGE_CURVE('',#2754,#2764,#754,.T.);
#3382=EDGE_CURVE('',#2765,#2766,#755,.T.);
#3383=EDGE_CURVE('',#2765,#2754,#756,.T.);
#3384=EDGE_CURVE('',#2764,#2766,#757,.T.);
#3385=EDGE_CURVE('',#2767,#2768,#1995,.T.);
#3386=EDGE_CURVE('',#2713,#2768,#1996,.T.);
#3387=EDGE_CURVE('',#2769,#2712,#1997,.T.);
#3388=EDGE_CURVE('',#2769,#2765,#1998,.T.);
#3389=EDGE_CURVE('',#2766,#2770,#1999,.T.);
#3390=EDGE_CURVE('',#2770,#2771,#2000,.T.);
#3391=EDGE_CURVE('',#2772,#2771,#2001,.T.);
#3392=EDGE_CURVE('',#2772,#2773,#2002,.T.);
#3393=EDGE_CURVE('',#2773,#2774,#2003,.T.);
#3394=EDGE_CURVE('',#2774,#2767,#758,.T.);
#3395=EDGE_CURVE('',#2775,#2775,#759,.T.);
#3396=EDGE_CURVE('',#2775,#2738,#2004,.T.);
#3397=EDGE_CURVE('',#2721,#2767,#760,.T.);
#3398=EDGE_CURVE('',#2720,#2768,#105,.T.);
#3399=EDGE_CURVE('',#2714,#2768,#2005,.T.);
#3400=EDGE_CURVE('',#2734,#2715,#2006,.T.);
#3401=EDGE_CURVE('',#2737,#2709,#2007,.T.);
#3402=EDGE_CURVE('',#2711,#2769,#2008,.T.);
#3403=EDGE_CURVE('',#2709,#2759,#761,.T.);
#3404=EDGE_CURVE('',#2710,#2758,#762,.T.);
#3405=EDGE_CURVE('',#2711,#2757,#763,.T.);
#3406=EDGE_CURVE('',#2756,#2769,#106,.T.);
#3407=EDGE_CURVE('',#2774,#2776,#764,.T.);
#3408=EDGE_CURVE('',#2776,#2721,#765,.T.);
#3409=EDGE_CURVE('',#2776,#2777,#2009,.T.);
#3410=EDGE_CURVE('',#2777,#2778,#2010,.T.);
#3411=EDGE_CURVE('',#2722,#2778,#766,.T.);
#3412=EDGE_CURVE('',#2777,#2779,#767,.T.);
#3413=EDGE_CURVE('',#2780,#2776,#2011,.T.);
#3414=EDGE_CURVE('',#2781,#2780,#2012,.T.);
#3415=EDGE_CURVE('',#2778,#2781,#2013,.T.);
#3416=EDGE_CURVE('',#2779,#2777,#768,.T.);
#3417=EDGE_CURVE('',#2782,#2782,#769,.T.);
#3418=EDGE_CURVE('',#2782,#2779,#2014,.T.);
#3419=EDGE_CURVE('',#2743,#2783,#770,.T.);
#3420=EDGE_CURVE('',#2784,#2783,#2015,.T.);
#3421=EDGE_CURVE('',#2784,#2772,#771,.T.);
#3422=EDGE_CURVE('',#2771,#2785,#772,.T.);
#3423=EDGE_CURVE('',#2785,#2786,#2016,.T.);
#3424=EDGE_CURVE('',#2786,#2744,#773,.T.);
#3425=EDGE_CURVE('',#2787,#2787,#774,.T.);
#3426=EDGE_CURVE('',#2787,#2763,#2017,.T.);
#3427=EDGE_CURVE('',#2763,#2763,#775,.T.);
#3428=EDGE_CURVE('',#2788,#2762,#2018,.T.);
#3429=EDGE_CURVE('',#2788,#2789,#2019,.T.);
#3430=EDGE_CURVE('',#2764,#2789,#2020,.T.);
#3431=EDGE_CURVE('',#2770,#2789,#776,.T.);
#3432=EDGE_CURVE('',#2790,#2770,#777,.T.);
#3433=EDGE_CURVE('',#2789,#2790,#778,.T.);
#3434=EDGE_CURVE('',#2790,#2785,#2021,.T.);
#3435=EDGE_CURVE('',#2786,#2791,#2022,.T.);
#3436=EDGE_CURVE('',#2791,#2790,#2023,.T.);
#3437=EDGE_CURVE('',#2745,#2791,#779,.T.);
#3438=EDGE_CURVE('',#2788,#2745,#780,.T.);
#3439=EDGE_CURVE('',#2791,#2788,#781,.T.);
#3440=EDGE_CURVE('',#2746,#2762,#782,.T.);
#3441=EDGE_CURVE('',#2792,#2742,#783,.T.);
#3442=EDGE_CURVE('',#2792,#2783,#2024,.T.);
#3443=EDGE_CURVE('',#2792,#2793,#2025,.T.);
#3444=EDGE_CURVE('',#2784,#2793,#2026,.T.);
#3445=EDGE_CURVE('',#2773,#2793,#784,.T.);
#3446=EDGE_CURVE('',#2793,#2780,#785,.T.);
#3447=EDGE_CURVE('',#2780,#2773,#786,.T.);
#3448=EDGE_CURVE('',#2781,#2792,#787,.T.);
#3449=EDGE_CURVE('',#2742,#2781,#788,.T.);
#3450=EDGE_CURVE('',#2778,#2741,#789,.T.);
#3451=EDGE_CURVE('',#2725,#2761,#2027,.T.);
#3452=EDGE_CURVE('',#2726,#2760,#2028,.T.);
#3453=EDGE_CURVE('',#2794,#2794,#790,.T.);
#3454=EDGE_CURVE('',#2794,#2795,#2029,.T.);
#3455=EDGE_CURVE('',#2795,#2795,#791,.T.);
#3456=EDGE_CURVE('',#2796,#2796,#792,.T.);
#3457=EDGE_CURVE('',#2797,#2797,#793,.T.);
#3458=EDGE_CURVE('',#2797,#2798,#2030,.T.);
#3459=EDGE_CURVE('',#2798,#2798,#794,.T.);
#3460=EDGE_CURVE('',#2799,#2799,#795,.T.);
#3461=EDGE_CURVE('',#2800,#2801,#2031,.T.);
#3462=EDGE_CURVE('',#2802,#2800,#2032,.T.);
#3463=EDGE_CURVE('',#2803,#2802,#2033,.T.);
#3464=EDGE_CURVE('',#2804,#2803,#2034,.T.);
#3465=EDGE_CURVE('',#2805,#2804,#2035,.T.);
#3466=EDGE_CURVE('',#2801,#2805,#2036,.T.);
#3467=EDGE_CURVE('',#2806,#2806,#796,.T.);
#3468=EDGE_CURVE('',#2801,#2807,#2037,.T.);
#3469=EDGE_CURVE('',#2808,#2807,#2038,.T.);
#3470=EDGE_CURVE('',#2800,#2808,#2039,.T.);
#3471=EDGE_CURVE('',#2809,#2808,#2040,.T.);
#3472=EDGE_CURVE('',#2802,#2809,#2041,.T.);
#3473=EDGE_CURVE('',#2810,#2809,#2042,.T.);
#3474=EDGE_CURVE('',#2803,#2810,#2043,.T.);
#3475=EDGE_CURVE('',#2811,#2810,#2044,.T.);
#3476=EDGE_CURVE('',#2804,#2811,#2045,.T.);
#3477=EDGE_CURVE('',#2812,#2811,#2046,.T.);
#3478=EDGE_CURVE('',#2805,#2812,#2047,.T.);
#3479=EDGE_CURVE('',#2807,#2812,#2048,.T.);
#3480=EDGE_CURVE('',#2813,#2813,#797,.T.);
#3481=EDGE_CURVE('',#2806,#2814,#2049,.T.);
#3482=EDGE_CURVE('',#2814,#2814,#798,.T.);
#3483=EDGE_CURVE('',#2815,#2815,#799,.T.);
#3484=EDGE_CURVE('',#2815,#2813,#2050,.T.);
#3485=EDGE_CURVE('',#2816,#2816,#800,.T.);
#3486=EDGE_CURVE('',#2816,#2817,#2051,.T.);
#3487=EDGE_CURVE('',#2817,#2817,#801,.T.);
#3488=EDGE_CURVE('',#2818,#2818,#802,.T.);
#3489=EDGE_CURVE('',#2818,#2819,#2052,.T.);
#3490=EDGE_CURVE('',#2819,#2819,#803,.T.);
#3491=EDGE_CURVE('',#2820,#2820,#804,.T.);
#3492=EDGE_CURVE('',#2821,#2821,#805,.T.);
#3493=EDGE_CURVE('',#2821,#2822,#2053,.T.);
#3494=EDGE_CURVE('',#2822,#2822,#806,.T.);
#3495=EDGE_CURVE('',#2823,#2823,#807,.T.);
#3496=EDGE_CURVE('',#2824,#2824,#808,.T.);
#3497=EDGE_CURVE('',#2825,#2825,#809,.T.);
#3498=EDGE_CURVE('',#2824,#2826,#2054,.T.);
#3499=EDGE_CURVE('',#2826,#2826,#810,.T.);
#3500=EDGE_CURVE('',#2827,#2828,#170,.T.);
#3501=EDGE_CURVE('',#2828,#2827,#171,.T.);
#3502=EDGE_CURVE('',#2829,#2829,#172,.T.);
#3503=EDGE_CURVE('',#2830,#2830,#811,.T.);
#3504=EDGE_CURVE('',#2831,#2831,#812,.T.);
#3505=EDGE_CURVE('',#2832,#2832,#813,.T.);
#3506=EDGE_CURVE('',#2833,#2833,#814,.T.);
#3507=EDGE_CURVE('',#2834,#2834,#815,.T.);
#3508=EDGE_CURVE('',#2835,#2835,#816,.T.);
#3509=EDGE_CURVE('',#2836,#2836,#817,.T.);
#3510=EDGE_CURVE('',#2837,#2837,#818,.T.);
#3511=EDGE_CURVE('',#2838,#2838,#819,.T.);
#3512=EDGE_CURVE('',#2830,#2839,#2055,.T.);
#3513=EDGE_CURVE('',#2839,#2839,#820,.T.);
#3514=EDGE_CURVE('',#2840,#2840,#821,.T.);
#3515=EDGE_CURVE('',#2840,#2841,#2056,.T.);
#3516=EDGE_CURVE('',#2841,#2841,#822,.T.);
#3517=EDGE_CURVE('',#2842,#2842,#823,.T.);
#3518=EDGE_CURVE('',#2842,#2843,#2057,.T.);
#3519=EDGE_CURVE('',#2843,#2843,#824,.T.);
#3520=EDGE_CURVE('',#2844,#2844,#825,.T.);
#3521=EDGE_CURVE('',#2845,#2845,#826,.T.);
#3522=EDGE_CURVE('',#2846,#2846,#827,.T.);
#3523=EDGE_CURVE('',#2847,#2847,#828,.T.);
#3524=EDGE_CURVE('',#2848,#2848,#829,.T.);
#3525=EDGE_CURVE('',#2849,#2849,#830,.T.);
#3526=EDGE_CURVE('',#2850,#2850,#831,.T.);
#3527=EDGE_CURVE('',#2851,#2851,#832,.T.);
#3528=EDGE_CURVE('',#2852,#2852,#833,.T.);
#3529=EDGE_CURVE('',#2844,#2853,#2058,.T.);
#3530=EDGE_CURVE('',#2853,#2853,#834,.T.);
#3531=EDGE_CURVE('',#2854,#2854,#835,.T.);
#3532=EDGE_CURVE('',#2854,#2825,#2059,.T.);
#3533=EDGE_CURVE('',#2855,#2855,#173,.T.);
#3534=EDGE_CURVE('',#2856,#2857,#174,.T.);
#3535=EDGE_CURVE('',#2857,#2856,#175,.T.);
#3536=EDGE_CURVE('',#2857,#2829,#2060,.T.);
#3537=EDGE_CURVE('',#2828,#2855,#2061,.T.);
#3538=EDGE_CURVE('',#2831,#2845,#2062,.T.);
#3539=EDGE_CURVE('',#2832,#2846,#2063,.T.);
#3540=EDGE_CURVE('',#2833,#2847,#2064,.T.);
#3541=EDGE_CURVE('',#2834,#2848,#2065,.T.);
#3542=EDGE_CURVE('',#2835,#2849,#2066,.T.);
#3543=EDGE_CURVE('',#2836,#2850,#2067,.T.);
#3544=EDGE_CURVE('',#2837,#2851,#2068,.T.);
#3545=EDGE_CURVE('',#2838,#2852,#2069,.T.);
#3546=EDGE_CURVE('',#2858,#2858,#836,.T.);
#3547=EDGE_CURVE('',#2858,#2859,#2070,.T.);
#3548=EDGE_CURVE('',#2859,#2860,#176,.F.);
#3549=EDGE_CURVE('',#2860,#2861,#837,.T.);
#3550=EDGE_CURVE('',#2861,#2862,#177,.F.);
#3551=EDGE_CURVE('',#2862,#2863,#178,.F.);
#3552=EDGE_CURVE('',#2864,#2863,#2071,.T.);
#3553=EDGE_CURVE('',#2865,#2864,#838,.T.);
#3554=EDGE_CURVE('',#2866,#2865,#2072,.T.);
#3555=EDGE_CURVE('',#2866,#2859,#179,.F.);
#3556=EDGE_CURVE('',#2867,#2868,#839,.T.);
#3557=EDGE_CURVE('',#2868,#2869,#2073,.T.);
#3558=EDGE_CURVE('',#2869,#2870,#840,.T.);
#3559=EDGE_CURVE('',#2870,#2867,#2074,.T.);
#3560=EDGE_CURVE('',#2871,#2871,#841,.T.);
#3561=EDGE_CURVE('',#2872,#2872,#842,.T.);
#3562=EDGE_CURVE('',#2872,#2873,#2075,.T.);
#3563=EDGE_CURVE('',#2873,#2873,#843,.T.);
#3564=EDGE_CURVE('',#2874,#2875,#844,.T.);
#3565=EDGE_CURVE('',#2874,#2876,#2076,.T.);
#3566=EDGE_CURVE('',#2876,#2877,#845,.T.);
#3567=EDGE_CURVE('',#2877,#2875,#2077,.T.);
#3568=EDGE_CURVE('',#2878,#2875,#180,.T.);
#3569=EDGE_CURVE('',#2861,#2878,#181,.T.);
#3570=EDGE_CURVE('',#2879,#2860,#182,.T.);
#3571=EDGE_CURVE('',#2874,#2879,#183,.T.);
#3572=EDGE_CURVE('',#2880,#2881,#2078,.T.);
#3573=EDGE_CURVE('',#2880,#2876,#2079,.T.);
#3574=EDGE_CURVE('',#2879,#2882,#107,.T.);
#3575=EDGE_CURVE('',#2881,#2882,#2080,.T.);
#3576=EDGE_CURVE('',#2870,#2880,#846,.T.);
#3577=EDGE_CURVE('',#2867,#2881,#847,.T.);
#3578=EDGE_CURVE('',#2881,#2865,#848,.T.);
#3579=EDGE_CURVE('',#2868,#2864,#849,.T.);
#3580=EDGE_CURVE('',#2864,#2883,#2081,.T.);
#3581=EDGE_CURVE('',#2869,#2883,#850,.T.);
#3582=EDGE_CURVE('',#2883,#2880,#851,.T.);
#3583=EDGE_CURVE('',#2883,#2877,#2082,.T.);
#3584=EDGE_CURVE('',#2878,#2863,#108,.T.);
#3585=EDGE_CURVE('',#2882,#2866,#184,.F.);
#3586=EDGE_CURVE('',#2859,#2884,#2083,.T.);
#3587=EDGE_CURVE('',#2885,#2884,#185,.T.);
#3588=EDGE_CURVE('',#2884,#2885,#186,.T.);
#3589=EDGE_CURVE('',#2886,#2887,#187,.T.);
#3590=EDGE_CURVE('',#2887,#2886,#188,.T.);
#3591=EDGE_CURVE('',#2887,#2862,#2084,.T.);
#3592=EDGE_CURVE('',#2871,#2885,#2085,.T.);
#3593=EDGE_CURVE('',#2884,#2888,#2086,.T.);
#3594=EDGE_CURVE('',#2888,#2888,#852,.T.);
#3595=EDGE_CURVE('',#2889,#2889,#853,.T.);
#3596=EDGE_CURVE('',#2889,#2890,#2087,.T.);
#3597=EDGE_CURVE('',#2890,#2890,#854,.T.);
#3598=EDGE_CURVE('',#2891,#2891,#855,.T.);
#3599=EDGE_CURVE('',#2892,#2892,#856,.T.);
#3600=EDGE_CURVE('',#2892,#2893,#2088,.T.);
#3601=EDGE_CURVE('',#2893,#2893,#857,.T.);
#3602=EDGE_CURVE('',#2894,#2894,#858,.T.);
#3603=EDGE_CURVE('',#2894,#2895,#2089,.T.);
#3604=EDGE_CURVE('',#2895,#2895,#859,.T.);
#3605=EDGE_CURVE('',#2896,#2896,#860,.T.);
#3606=EDGE_CURVE('',#2896,#2897,#2090,.T.);
#3607=EDGE_CURVE('',#2897,#2898,#861,.T.);
#3608=EDGE_CURVE('',#2898,#2899,#2091,.T.);
#3609=EDGE_CURVE('',#2899,#2900,#862,.T.);
#3610=EDGE_CURVE('',#2901,#2900,#2092,.T.);
#3611=EDGE_CURVE('',#2902,#2901,#863,.T.);
#3612=EDGE_CURVE('',#2902,#2903,#2093,.T.);
#3613=EDGE_CURVE('',#2903,#2904,#864,.T.);
#3614=EDGE_CURVE('',#2905,#2904,#2094,.T.);
#3615=EDGE_CURVE('',#2905,#2897,#865,.T.);
#3616=EDGE_CURVE('',#2903,#2900,#2095,.T.);
#3617=EDGE_CURVE('',#2901,#2902,#2096,.T.);
#3618=EDGE_CURVE('',#2904,#2899,#2097,.T.);
#3619=EDGE_CURVE('',#2898,#2905,#2098,.T.);
#3620=EDGE_CURVE('',#2906,#2906,#866,.T.);
#3621=EDGE_CURVE('',#2906,#2907,#2099,.T.);
#3622=EDGE_CURVE('',#2907,#2907,#867,.T.);
#3623=EDGE_CURVE('',#2908,#2908,#868,.T.);
#3624=EDGE_CURVE('',#2909,#2909,#869,.T.);
#3625=EDGE_CURVE('',#2910,#2910,#870,.T.);
#3626=EDGE_CURVE('',#2910,#2911,#2100,.T.);
#3627=EDGE_CURVE('',#2912,#2911,#189,.T.);
#3628=EDGE_CURVE('',#2912,#2913,#2101,.T.);
#3629=EDGE_CURVE('',#2914,#2913,#190,.T.);
#3630=EDGE_CURVE('',#2914,#2909,#2102,.T.);
#3631=EDGE_CURVE('',#2913,#2914,#191,.T.);
#3632=EDGE_CURVE('',#2911,#2912,#192,.T.);
#3633=EDGE_CURVE('',#2915,#2916,#193,.T.);
#3634=EDGE_CURVE('',#2916,#2915,#194,.T.);
#3635=EDGE_CURVE('',#2917,#2917,#195,.T.);
#3636=EDGE_CURVE('',#2918,#2918,#871,.T.);
#3637=EDGE_CURVE('',#2918,#2916,#2103,.T.);
#3638=EDGE_CURVE('',#2911,#2919,#2104,.T.);
#3639=EDGE_CURVE('',#2919,#2919,#872,.T.);
#3640=EDGE_CURVE('',#2913,#2920,#2105,.T.);
#3641=EDGE_CURVE('',#2920,#2920,#873,.T.);
#3642=EDGE_CURVE('',#2921,#2921,#874,.T.);
#3643=EDGE_CURVE('',#2921,#2917,#2106,.T.);
#3644=EDGE_CURVE('',#2922,#2923,#2107,.T.);
#3645=EDGE_CURVE('',#2924,#2923,#2108,.T.);
#3646=EDGE_CURVE('',#2924,#2925,#2109,.T.);
#3647=EDGE_CURVE('',#2925,#2922,#875,.T.);
#3648=EDGE_CURVE('',#2923,#2926,#876,.T.);
#3649=EDGE_CURVE('',#2922,#2927,#877,.T.);
#3650=EDGE_CURVE('',#2927,#2926,#2110,.T.);
#3651=EDGE_CURVE('',#2926,#2928,#2111,.T.);
#3652=EDGE_CURVE('',#2928,#2929,#2112,.T.);
#3653=EDGE_CURVE('',#2929,#2930,#2113,.T.);
#3654=EDGE_CURVE('',#2930,#2924,#878,.T.);
#3655=EDGE_CURVE('',#2931,#2931,#879,.T.);
#3656=EDGE_CURVE('',#2932,#2932,#880,.T.);
#3657=EDGE_CURVE('',#2933,#2934,#196,.T.);
#3658=EDGE_CURVE('',#2934,#2933,#197,.T.);
#3659=EDGE_CURVE('',#2934,#2932,#2114,.T.);
#3660=EDGE_CURVE('',#2935,#2935,#881,.T.);
#3661=EDGE_CURVE('',#2935,#2936,#2115,.T.);
#3662=EDGE_CURVE('',#2936,#2936,#882,.T.);
#3663=EDGE_CURVE('',#2937,#2938,#198,.T.);
#3664=EDGE_CURVE('',#2938,#2937,#199,.T.);
#3665=EDGE_CURVE('',#2939,#2939,#883,.T.);
#3666=EDGE_CURVE('',#2940,#2940,#884,.T.);
#3667=EDGE_CURVE('',#2941,#2941,#885,.T.);
#3668=EDGE_CURVE('',#2942,#2942,#886,.T.);
#3669=EDGE_CURVE('',#2939,#2943,#2116,.T.);
#3670=EDGE_CURVE('',#2943,#2944,#887,.T.);
#3671=EDGE_CURVE('',#2944,#2943,#888,.T.);
#3672=EDGE_CURVE('',#2944,#2945,#889,.T.);
#3673=EDGE_CURVE('',#2945,#2945,#890,.T.);
#3674=EDGE_CURVE('',#2946,#2946,#891,.T.);
#3675=EDGE_CURVE('',#2947,#2947,#892,.T.);
#3676=EDGE_CURVE('',#2948,#2948,#893,.T.);
#3677=EDGE_CURVE('',#2949,#2949,#894,.T.);
#3678=EDGE_CURVE('',#2949,#2940,#2117,.T.);
#3679=EDGE_CURVE('',#2946,#2941,#2118,.T.);
#3680=EDGE_CURVE('',#2947,#2942,#2119,.T.);
#3681=EDGE_CURVE('',#2948,#2950,#895,.T.);
#3682=EDGE_CURVE('',#2951,#2950,#896,.T.);
#3683=EDGE_CURVE('',#2950,#2951,#897,.T.);
#3684=EDGE_CURVE('',#2951,#2952,#2120,.T.);
#3685=EDGE_CURVE('',#2952,#2953,#898,.T.);
#3686=EDGE_CURVE('',#2953,#2927,#2121,.T.);
#3687=EDGE_CURVE('',#2954,#2927,#899,.T.);
#3688=EDGE_CURVE('',#2954,#2952,#2122,.T.);
#3689=EDGE_CURVE('',#2955,#2955,#200,.T.);
#3690=EDGE_CURVE('',#2938,#2955,#2123,.T.);
#3691=EDGE_CURVE('',#2956,#2957,#900,.T.);
#3692=EDGE_CURVE('',#2953,#2956,#201,.T.);
#3693=EDGE_CURVE('',#2957,#2952,#202,.T.);
#3694=EDGE_CURVE('',#2929,#2957,#2124,.T.);
#3695=EDGE_CURVE('',#2928,#2956,#2125,.T.);
#3696=EDGE_CURVE('',#2925,#2954,#901,.T.);
#3697=EDGE_CURVE('',#2930,#2954,#2126,.T.);
#3698=EDGE_CURVE('',#2958,#2958,#902,.T.);
#3699=EDGE_CURVE('',#2958,#2931,#2127,.T.);
#3700=EDGE_CURVE('',#2959,#2959,#903,.T.);
#3701=EDGE_CURVE('',#2959,#2960,#2128,.T.);
#3702=EDGE_CURVE('',#2960,#2960,#904,.T.);
#3703=EDGE_CURVE('',#2961,#2961,#905,.T.);
#3704=EDGE_CURVE('',#2962,#2962,#906,.T.);
#3705=EDGE_CURVE('',#2962,#2963,#2129,.T.);
#3706=EDGE_CURVE('',#2963,#2963,#907,.T.);
#3707=EDGE_CURVE('',#2964,#2964,#908,.T.);
#3708=EDGE_CURVE('',#2965,#2965,#909,.T.);
#3709=EDGE_CURVE('',#2965,#2966,#2130,.T.);
#3710=EDGE_CURVE('',#2966,#2966,#910,.T.);
#3711=EDGE_CURVE('',#2967,#2967,#911,.T.);
#3712=EDGE_CURVE('',#2968,#2968,#912,.T.);
#3713=EDGE_CURVE('',#2968,#2969,#2131,.T.);
#3714=EDGE_CURVE('',#2969,#2969,#913,.T.);
#3715=EDGE_CURVE('',#2970,#2970,#914,.T.);
#3716=EDGE_CURVE('',#2971,#2971,#915,.T.);
#3717=EDGE_CURVE('',#2971,#2972,#2132,.T.);
#3718=EDGE_CURVE('',#2972,#2972,#916,.T.);
#3719=EDGE_CURVE('',#2973,#2973,#917,.T.);
#3720=EDGE_CURVE('',#2974,#2974,#918,.T.);
#3721=EDGE_CURVE('',#2975,#2975,#919,.T.);
#3722=EDGE_CURVE('',#2976,#2976,#920,.T.);
#3723=EDGE_CURVE('',#2977,#2977,#921,.T.);
#3724=EDGE_CURVE('',#2978,#2978,#922,.T.);
#3725=EDGE_CURVE('',#2975,#2979,#2133,.T.);
#3726=EDGE_CURVE('',#2979,#2979,#923,.T.);
#3727=EDGE_CURVE('',#2980,#2980,#924,.T.);
#3728=EDGE_CURVE('',#2980,#2981,#2134,.T.);
#3729=EDGE_CURVE('',#2981,#2981,#925,.T.);
#3730=EDGE_CURVE('',#2982,#2982,#926,.T.);
#3731=EDGE_CURVE('',#2982,#2983,#927,.T.);
#3732=EDGE_CURVE('',#2983,#2984,#928,.T.);
#3733=EDGE_CURVE('',#2984,#2983,#929,.T.);
#3734=EDGE_CURVE('',#2984,#2985,#2135,.T.);
#3735=EDGE_CURVE('',#2985,#2985,#930,.T.);
#3736=EDGE_CURVE('',#2986,#2986,#931,.T.);
#3737=EDGE_CURVE('',#2987,#2987,#932,.T.);
#3738=EDGE_CURVE('',#2988,#2988,#933,.T.);
#3739=EDGE_CURVE('',#2989,#2989,#934,.T.);
#3740=EDGE_CURVE('',#2976,#2987,#2136,.T.);
#3741=EDGE_CURVE('',#2977,#2988,#2137,.T.);
#3742=EDGE_CURVE('',#2978,#2989,#2138,.T.);
#3743=EDGE_CURVE('',#2986,#2990,#935,.T.);
#3744=EDGE_CURVE('',#2990,#2991,#936,.T.);
#3745=EDGE_CURVE('',#2991,#2990,#937,.T.);
#3746=EDGE_CURVE('',#2991,#2974,#2139,.T.);
#3747=EDGE_CURVE('',#2992,#2993,#203,.T.);
#3748=EDGE_CURVE('',#2993,#2992,#204,.T.);
#3749=EDGE_CURVE('',#2993,#2994,#205,.T.);
#3750=EDGE_CURVE('',#2995,#2994,#206,.T.);
#3751=EDGE_CURVE('',#2992,#2995,#207,.T.);
#3752=EDGE_CURVE('',#2994,#2995,#208,.T.);
#3753=EDGE_CURVE('',#2995,#2996,#209,.T.);
#3754=EDGE_CURVE('',#2997,#2996,#210,.T.);
#3755=EDGE_CURVE('',#2994,#2997,#211,.T.);
#3756=EDGE_CURVE('',#2996,#2997,#212,.T.);
#3757=EDGE_CURVE('',#2997,#2998,#213,.T.);
#3758=EDGE_CURVE('',#2999,#2998,#214,.T.);
#3759=EDGE_CURVE('',#2996,#2999,#215,.T.);
#3760=EDGE_CURVE('',#2998,#2999,#216,.T.);
#3761=EDGE_CURVE('',#3000,#3001,#2140,.T.);
#3762=EDGE_CURVE('',#3002,#3000,#2141,.T.);
#3763=EDGE_CURVE('',#3003,#3002,#2142,.T.);
#3764=EDGE_CURVE('',#3004,#3003,#2143,.T.);
#3765=EDGE_CURVE('',#3005,#3004,#2144,.T.);
#3766=EDGE_CURVE('',#3001,#3005,#2145,.T.);
#3767=EDGE_CURVE('',#3006,#3006,#938,.T.);
#3768=EDGE_CURVE('',#3006,#3007,#2146,.T.);
#3769=EDGE_CURVE('',#3007,#3007,#939,.T.);
#3770=EDGE_CURVE('',#3008,#3009,#2147,.T.);
#3771=EDGE_CURVE('',#3009,#3010,#2148,.T.);
#3772=EDGE_CURVE('',#3010,#3011,#2149,.T.);
#3773=EDGE_CURVE('',#3011,#3012,#2150,.T.);
#3774=EDGE_CURVE('',#3012,#3013,#2151,.T.);
#3775=EDGE_CURVE('',#3013,#3008,#2152,.T.);
#3776=EDGE_CURVE('',#3001,#3009,#2153,.T.);
#3777=EDGE_CURVE('',#3000,#3008,#2154,.T.);
#3778=EDGE_CURVE('',#3002,#3013,#2155,.T.);
#3779=EDGE_CURVE('',#3003,#3012,#2156,.T.);
#3780=EDGE_CURVE('',#3004,#3011,#2157,.T.);
#3781=EDGE_CURVE('',#3005,#3010,#2158,.T.);
#3782=EDGE_CURVE('',#3014,#3014,#940,.T.);
#3783=EDGE_CURVE('',#3014,#3015,#2159,.T.);
#3784=EDGE_CURVE('',#3015,#3015,#941,.T.);
#3785=EDGE_CURVE('',#3016,#3016,#942,.T.);
#3786=EDGE_CURVE('',#3017,#3018,#943,.T.);
#3787=EDGE_CURVE('',#3018,#3019,#944,.T.);
#3788=EDGE_CURVE('',#3019,#3020,#945,.T.);
#3789=EDGE_CURVE('',#3020,#3021,#2160,.T.);
#3790=EDGE_CURVE('',#3021,#3022,#946,.T.);
#3791=EDGE_CURVE('',#3022,#3023,#947,.T.);
#3792=EDGE_CURVE('',#3023,#3024,#948,.T.);
#3793=EDGE_CURVE('',#3024,#3017,#2161,.T.);
#3794=EDGE_CURVE('',#3025,#3026,#949,.T.);
#3795=EDGE_CURVE('',#3018,#3025,#2162,.T.);
#3796=EDGE_CURVE('',#3017,#3026,#2163,.T.);
#3797=EDGE_CURVE('',#3027,#3027,#950,.T.);
#3798=EDGE_CURVE('',#3028,#3026,#2164,.T.);
#3799=EDGE_CURVE('',#3029,#3028,#951,.T.);
#3800=EDGE_CURVE('',#3030,#3029,#2165,.T.);
#3801=EDGE_CURVE('',#3030,#3031,#952,.T.);
#3802=EDGE_CURVE('',#3025,#3031,#953,.T.);
#3803=EDGE_CURVE('',#3032,#3033,#954,.T.);
#3804=EDGE_CURVE('',#3034,#3033,#2166,.T.);
#3805=EDGE_CURVE('',#3035,#3034,#955,.T.);
#3806=EDGE_CURVE('',#3036,#3035,#2167,.T.);
#3807=EDGE_CURVE('',#3036,#3037,#956,.T.);
#3808=EDGE_CURVE('',#3032,#3037,#957,.T.);
#3809=EDGE_CURVE('',#3027,#3038,#2168,.T.);
#3810=EDGE_CURVE('',#3038,#3038,#958,.T.);
#3811=EDGE_CURVE('',#3039,#3039,#959,.T.);
#3812=EDGE_CURVE('',#3039,#3040,#2169,.T.);
#3813=EDGE_CURVE('',#3040,#3041,#960,.T.);
#3814=EDGE_CURVE('',#3041,#3040,#961,.T.);
#3815=EDGE_CURVE('',#3028,#3040,#217,.T.);
#3816=EDGE_CURVE('',#3041,#3029,#218,.T.);
#3817=EDGE_CURVE('',#3020,#3030,#2170,.T.);
#3818=EDGE_CURVE('',#3034,#3041,#219,.T.);
#3819=EDGE_CURVE('',#3021,#3033,#2171,.T.);
#3820=EDGE_CURVE('',#3042,#3042,#962,.T.);
#3821=EDGE_CURVE('',#3042,#3043,#2172,.T.);
#3822=EDGE_CURVE('',#3043,#3043,#963,.T.);
#3823=EDGE_CURVE('',#3024,#3036,#2173,.T.);
#3824=EDGE_CURVE('',#3040,#3035,#220,.T.);
#3825=EDGE_CURVE('',#3023,#3037,#2174,.T.);
#3826=EDGE_CURVE('',#3022,#3032,#2175,.T.);
#3827=EDGE_CURVE('',#3019,#3031,#2176,.T.);
#3828=EDGE_CURVE('',#3044,#3044,#964,.T.);
#3829=EDGE_CURVE('',#3044,#3045,#2177,.T.);
#3830=EDGE_CURVE('',#3045,#3045,#965,.T.);
#3831=EDGE_CURVE('',#3046,#3046,#966,.T.);
#3832=EDGE_CURVE('',#3047,#3047,#967,.T.);
#3833=EDGE_CURVE('',#3048,#3048,#968,.T.);
#3834=EDGE_CURVE('',#3049,#3049,#969,.T.);
#3835=EDGE_CURVE('',#3049,#3047,#2178,.T.);
#3836=EDGE_CURVE('',#3050,#3050,#970,.T.);
#3837=EDGE_CURVE('',#3050,#3048,#2179,.T.);
#3838=EDGE_CURVE('',#3051,#3051,#971,.T.);
#3839=EDGE_CURVE('',#3051,#3052,#2180,.T.);
#3840=EDGE_CURVE('',#3052,#3052,#972,.T.);
#3841=EDGE_CURVE('',#3053,#3053,#973,.T.);
#3842=EDGE_CURVE('',#3054,#3054,#974,.T.);
#3843=EDGE_CURVE('',#3054,#3055,#2181,.T.);
#3844=EDGE_CURVE('',#3055,#3055,#975,.T.);
#3845=EDGE_CURVE('',#3056,#3056,#976,.T.);
#3846=EDGE_CURVE('',#3057,#3057,#977,.T.);
#3847=EDGE_CURVE('',#3058,#3058,#978,.T.);
#3848=EDGE_CURVE('',#3058,#3059,#2182,.T.);
#3849=EDGE_CURVE('',#3059,#3059,#979,.T.);
#3850=EDGE_CURVE('',#3060,#3060,#980,.T.);
#3851=EDGE_CURVE('',#3060,#3061,#2183,.T.);
#3852=EDGE_CURVE('',#3061,#3061,#981,.T.);
#3853=EDGE_CURVE('',#3062,#3062,#982,.T.);
#3854=EDGE_CURVE('',#3062,#3063,#2184,.T.);
#3855=EDGE_CURVE('',#3063,#3063,#983,.T.);
#3856=EDGE_CURVE('',#3064,#3064,#984,.T.);
#3857=EDGE_CURVE('',#3064,#3057,#2185,.T.);
#3858=EDGE_CURVE('',#3065,#3065,#985,.T.);
#3859=EDGE_CURVE('',#3065,#3066,#2186,.T.);
#3860=EDGE_CURVE('',#3066,#3066,#986,.T.);
#3861=EDGE_CURVE('',#3067,#3067,#987,.T.);
#3862=EDGE_CURVE('',#3068,#3069,#988,.T.);
#3863=EDGE_CURVE('',#3070,#3068,#2187,.T.);
#3864=EDGE_CURVE('',#3071,#3070,#989,.T.);
#3865=EDGE_CURVE('',#3072,#3071,#2188,.T.);
#3866=EDGE_CURVE('',#3073,#3072,#990,.T.);
#3867=EDGE_CURVE('',#3074,#3073,#2189,.T.);
#3868=EDGE_CURVE('',#3075,#3074,#991,.T.);
#3869=EDGE_CURVE('',#3069,#3075,#2190,.T.);
#3870=EDGE_CURVE('',#3076,#3076,#992,.T.);
#3871=EDGE_CURVE('',#3077,#3077,#993,.T.);
#3872=EDGE_CURVE('',#3077,#3078,#2191,.T.);
#3873=EDGE_CURVE('',#3078,#3078,#994,.T.);
#3874=EDGE_CURVE('',#3079,#3080,#995,.T.);
#3875=EDGE_CURVE('',#3080,#3081,#2192,.T.);
#3876=EDGE_CURVE('',#3081,#3082,#996,.T.);
#3877=EDGE_CURVE('',#3082,#3083,#2193,.T.);
#3878=EDGE_CURVE('',#3083,#3084,#997,.T.);
#3879=EDGE_CURVE('',#3084,#3085,#2194,.T.);
#3880=EDGE_CURVE('',#3085,#3086,#998,.T.);
#3881=EDGE_CURVE('',#3086,#3079,#2195,.T.);
#3882=EDGE_CURVE('',#3087,#3087,#999,.T.);
#3883=EDGE_CURVE('',#3088,#3089,#1000,.T.);
#3884=EDGE_CURVE('',#3089,#3080,#2196,.T.);
#3885=EDGE_CURVE('',#3088,#3079,#2197,.T.);
#3886=EDGE_CURVE('',#3090,#3091,#1001,.T.);
#3887=EDGE_CURVE('',#3091,#3092,#2198,.T.);
#3888=EDGE_CURVE('',#3092,#3093,#1002,.T.);
#3889=EDGE_CURVE('',#3093,#3094,#2199,.T.);
#3890=EDGE_CURVE('',#3094,#3095,#1003,.T.);
#3891=EDGE_CURVE('',#3095,#3096,#2200,.T.);
#3892=EDGE_CURVE('',#3096,#3097,#1004,.T.);
#3893=EDGE_CURVE('',#3097,#3090,#2201,.T.);
#3894=EDGE_CURVE('',#3098,#3088,#2202,.T.);
#3895=EDGE_CURVE('',#3099,#3098,#1005,.T.);
#3896=EDGE_CURVE('',#3100,#3099,#2203,.T.);
#3897=EDGE_CURVE('',#3101,#3100,#1006,.T.);
#3898=EDGE_CURVE('',#3102,#3101,#2204,.T.);
#3899=EDGE_CURVE('',#3103,#3102,#1007,.T.);
#3900=EDGE_CURVE('',#3089,#3103,#2205,.T.);
#3901=EDGE_CURVE('',#3069,#3091,#2206,.T.);
#3902=EDGE_CURVE('',#3068,#3090,#2207,.T.);
#3903=EDGE_CURVE('',#3070,#3097,#2208,.T.);
#3904=EDGE_CURVE('',#3071,#3096,#2209,.T.);
#3905=EDGE_CURVE('',#3072,#3095,#2210,.T.);
#3906=EDGE_CURVE('',#3073,#3094,#2211,.T.);
#3907=EDGE_CURVE('',#3074,#3093,#2212,.T.);
#3908=EDGE_CURVE('',#3075,#3092,#2213,.T.);
#3909=EDGE_CURVE('',#3103,#3081,#2214,.T.);
#3910=EDGE_CURVE('',#3102,#3082,#2215,.T.);
#3911=EDGE_CURVE('',#3101,#3083,#2216,.T.);
#3912=EDGE_CURVE('',#3100,#3084,#2217,.T.);
#3913=EDGE_CURVE('',#3099,#3085,#2218,.T.);
#3914=EDGE_CURVE('',#3098,#3086,#2219,.T.);
#3915=EDGE_CURVE('',#3076,#3087,#2220,.T.);
#3916=ORIENTED_EDGE('',*,*,#3104,.T.);
#3917=ORIENTED_EDGE('',*,*,#3105,.F.);
#3918=ORIENTED_EDGE('',*,*,#3106,.F.);
#3919=ORIENTED_EDGE('',*,*,#3107,.F.);
#3920=ORIENTED_EDGE('',*,*,#3104,.F.);
#3921=ORIENTED_EDGE('',*,*,#3108,.F.);
#3922=ORIENTED_EDGE('',*,*,#3109,.T.);
#3923=ORIENTED_EDGE('',*,*,#3110,.T.);
#3924=ORIENTED_EDGE('',*,*,#3111,.T.);
#3925=ORIENTED_EDGE('',*,*,#3112,.T.);
#3926=ORIENTED_EDGE('',*,*,#3110,.F.);
#3927=ORIENTED_EDGE('',*,*,#3113,.F.);
#3928=ORIENTED_EDGE('',*,*,#3114,.T.);
#3929=ORIENTED_EDGE('',*,*,#3115,.F.);
#3930=ORIENTED_EDGE('',*,*,#3111,.F.);
#3931=ORIENTED_EDGE('',*,*,#3116,.T.);
#3932=ORIENTED_EDGE('',*,*,#3117,.F.);
#3933=ORIENTED_EDGE('',*,*,#3118,.T.);
#3934=ORIENTED_EDGE('',*,*,#3119,.F.);
#3935=ORIENTED_EDGE('',*,*,#3120,.F.);
#3936=ORIENTED_EDGE('',*,*,#3114,.F.);
#3937=ORIENTED_EDGE('',*,*,#3121,.T.);
#3938=ORIENTED_EDGE('',*,*,#3122,.T.);
#3939=ORIENTED_EDGE('',*,*,#3123,.T.);
#3940=ORIENTED_EDGE('',*,*,#3115,.T.);
#3941=ORIENTED_EDGE('',*,*,#3123,.F.);
#3942=ORIENTED_EDGE('',*,*,#3124,.F.);
#3943=ORIENTED_EDGE('',*,*,#3105,.T.);
#3944=ORIENTED_EDGE('',*,*,#3112,.F.);
#3945=ORIENTED_EDGE('',*,*,#3106,.T.);
#3946=ORIENTED_EDGE('',*,*,#3124,.T.);
#3947=ORIENTED_EDGE('',*,*,#3122,.F.);
#3948=ORIENTED_EDGE('',*,*,#3125,.F.);
#3949=ORIENTED_EDGE('',*,*,#3126,.T.);
#3950=ORIENTED_EDGE('',*,*,#3127,.T.);
#3951=ORIENTED_EDGE('',*,*,#3128,.T.);
#3952=ORIENTED_EDGE('',*,*,#3129,.T.);
#3953=ORIENTED_EDGE('',*,*,#3118,.F.);
#3954=ORIENTED_EDGE('',*,*,#3130,.T.);
#3955=ORIENTED_EDGE('',*,*,#3107,.T.);
#3956=ORIENTED_EDGE('',*,*,#3125,.T.);
#3957=ORIENTED_EDGE('',*,*,#3121,.F.);
#3958=ORIENTED_EDGE('',*,*,#3117,.T.);
#3959=ORIENTED_EDGE('',*,*,#3131,.T.);
#3960=ORIENTED_EDGE('',*,*,#3108,.T.);
#3961=ORIENTED_EDGE('',*,*,#3130,.F.);
#3962=ORIENTED_EDGE('',*,*,#3116,.F.);
#3963=ORIENTED_EDGE('',*,*,#3113,.T.);
#3964=ORIENTED_EDGE('',*,*,#3109,.F.);
#3965=ORIENTED_EDGE('',*,*,#3131,.F.);
#3966=ORIENTED_EDGE('',*,*,#3132,.F.);
#3967=ORIENTED_EDGE('',*,*,#3133,.F.);
#3968=ORIENTED_EDGE('',*,*,#3134,.F.);
#3969=ORIENTED_EDGE('',*,*,#3135,.F.);
#3970=ORIENTED_EDGE('',*,*,#3126,.F.);
#3971=ORIENTED_EDGE('',*,*,#3136,.T.);
#3972=ORIENTED_EDGE('',*,*,#3132,.T.);
#3973=ORIENTED_EDGE('',*,*,#3136,.F.);
#3974=ORIENTED_EDGE('',*,*,#3127,.F.);
#3975=ORIENTED_EDGE('',*,*,#3137,.T.);
#3976=ORIENTED_EDGE('',*,*,#3133,.T.);
#3977=ORIENTED_EDGE('',*,*,#3137,.F.);
#3978=ORIENTED_EDGE('',*,*,#3128,.F.);
#3979=ORIENTED_EDGE('',*,*,#3138,.T.);
#3980=ORIENTED_EDGE('',*,*,#3134,.T.);
#3981=ORIENTED_EDGE('',*,*,#3138,.F.);
#3982=ORIENTED_EDGE('',*,*,#3129,.F.);
#3983=ORIENTED_EDGE('',*,*,#3139,.T.);
#3984=ORIENTED_EDGE('',*,*,#3135,.T.);
#3985=ORIENTED_EDGE('',*,*,#3139,.F.);
#3986=ORIENTED_EDGE('',*,*,#3140,.F.);
#3987=ORIENTED_EDGE('',*,*,#3141,.T.);
#3988=ORIENTED_EDGE('',*,*,#3119,.T.);
#3989=ORIENTED_EDGE('',*,*,#3141,.F.);
#3990=ORIENTED_EDGE('',*,*,#3140,.T.);
#3991=ORIENTED_EDGE('',*,*,#3142,.T.);
#3992=ORIENTED_EDGE('',*,*,#3142,.F.);
#3993=ORIENTED_EDGE('',*,*,#3143,.T.);
#3994=ORIENTED_EDGE('',*,*,#3120,.T.);
#3995=ORIENTED_EDGE('',*,*,#3143,.F.);
#3996=ORIENTED_EDGE('',*,*,#3144,.F.);
#3997=ORIENTED_EDGE('',*,*,#3145,.F.);
#3998=ORIENTED_EDGE('',*,*,#3146,.F.);
#3999=ORIENTED_EDGE('',*,*,#3147,.F.);
#4000=ORIENTED_EDGE('',*,*,#3148,.F.);
#4001=ORIENTED_EDGE('',*,*,#3149,.F.);
#4002=ORIENTED_EDGE('',*,*,#3150,.F.);
#4003=ORIENTED_EDGE('',*,*,#3151,.F.);
#4004=ORIENTED_EDGE('',*,*,#3152,.F.);
#4005=ORIENTED_EDGE('',*,*,#3153,.F.);
#4006=ORIENTED_EDGE('',*,*,#3154,.F.);
#4007=ORIENTED_EDGE('',*,*,#3155,.F.);
#4008=ORIENTED_EDGE('',*,*,#3156,.F.);
#4009=ORIENTED_EDGE('',*,*,#3157,.F.);
#4010=ORIENTED_EDGE('',*,*,#3157,.T.);
#4011=ORIENTED_EDGE('',*,*,#3158,.T.);
#4012=ORIENTED_EDGE('',*,*,#3159,.F.);
#4013=ORIENTED_EDGE('',*,*,#3158,.F.);
#4014=ORIENTED_EDGE('',*,*,#3160,.T.);
#4015=ORIENTED_EDGE('',*,*,#3161,.T.);
#4016=ORIENTED_EDGE('',*,*,#3162,.T.);
#4017=ORIENTED_EDGE('',*,*,#3163,.T.);
#4018=ORIENTED_EDGE('',*,*,#3164,.T.);
#4019=ORIENTED_EDGE('',*,*,#3165,.T.);
#4020=ORIENTED_EDGE('',*,*,#3166,.T.);
#4021=ORIENTED_EDGE('',*,*,#3167,.T.);
#4022=ORIENTED_EDGE('',*,*,#3168,.T.);
#4023=ORIENTED_EDGE('',*,*,#3169,.T.);
#4024=ORIENTED_EDGE('',*,*,#3170,.T.);
#4025=ORIENTED_EDGE('',*,*,#3171,.T.);
#4026=ORIENTED_EDGE('',*,*,#3172,.T.);
#4027=ORIENTED_EDGE('',*,*,#3159,.T.);
#4028=ORIENTED_EDGE('',*,*,#3152,.T.);
#4029=ORIENTED_EDGE('',*,*,#3173,.T.);
#4030=ORIENTED_EDGE('',*,*,#3168,.F.);
#4031=ORIENTED_EDGE('',*,*,#3173,.F.);
#4032=ORIENTED_EDGE('',*,*,#3153,.T.);
#4033=ORIENTED_EDGE('',*,*,#3174,.T.);
#4034=ORIENTED_EDGE('',*,*,#3169,.F.);
#4035=ORIENTED_EDGE('',*,*,#3174,.F.);
#4036=ORIENTED_EDGE('',*,*,#3154,.T.);
#4037=ORIENTED_EDGE('',*,*,#3175,.T.);
#4038=ORIENTED_EDGE('',*,*,#3170,.F.);
#4039=ORIENTED_EDGE('',*,*,#3175,.F.);
#4040=ORIENTED_EDGE('',*,*,#3155,.T.);
#4041=ORIENTED_EDGE('',*,*,#3176,.T.);
#4042=ORIENTED_EDGE('',*,*,#3171,.F.);
#4043=ORIENTED_EDGE('',*,*,#3176,.F.);
#4044=ORIENTED_EDGE('',*,*,#3156,.T.);
#4045=ORIENTED_EDGE('',*,*,#3177,.T.);
#4046=ORIENTED_EDGE('',*,*,#3172,.F.);
#4047=ORIENTED_EDGE('',*,*,#3177,.F.);
#4048=ORIENTED_EDGE('',*,*,#3160,.F.);
#4049=ORIENTED_EDGE('',*,*,#3178,.T.);
#4050=ORIENTED_EDGE('',*,*,#3179,.T.);
#4051=ORIENTED_EDGE('',*,*,#3180,.F.);
#4052=ORIENTED_EDGE('',*,*,#3161,.F.);
#4053=ORIENTED_EDGE('',*,*,#3180,.T.);
#4054=ORIENTED_EDGE('',*,*,#3181,.T.);
#4055=ORIENTED_EDGE('',*,*,#3182,.F.);
#4056=ORIENTED_EDGE('',*,*,#3162,.F.);
#4057=ORIENTED_EDGE('',*,*,#3182,.T.);
#4058=ORIENTED_EDGE('',*,*,#3183,.T.);
#4059=ORIENTED_EDGE('',*,*,#3184,.F.);
#4060=ORIENTED_EDGE('',*,*,#3163,.F.);
#4061=ORIENTED_EDGE('',*,*,#3184,.T.);
#4062=ORIENTED_EDGE('',*,*,#3185,.T.);
#4063=ORIENTED_EDGE('',*,*,#3186,.F.);
#4064=ORIENTED_EDGE('',*,*,#3164,.F.);
#4065=ORIENTED_EDGE('',*,*,#3186,.T.);
#4066=ORIENTED_EDGE('',*,*,#3187,.T.);
#4067=ORIENTED_EDGE('',*,*,#3188,.F.);
#4068=ORIENTED_EDGE('',*,*,#3165,.F.);
#4069=ORIENTED_EDGE('',*,*,#3188,.T.);
#4070=ORIENTED_EDGE('',*,*,#3189,.T.);
#4071=ORIENTED_EDGE('',*,*,#3190,.F.);
#4072=ORIENTED_EDGE('',*,*,#3166,.F.);
#4073=ORIENTED_EDGE('',*,*,#3190,.T.);
#4074=ORIENTED_EDGE('',*,*,#3191,.T.);
#4075=ORIENTED_EDGE('',*,*,#3192,.F.);
#4076=ORIENTED_EDGE('',*,*,#3167,.F.);
#4077=ORIENTED_EDGE('',*,*,#3192,.T.);
#4078=ORIENTED_EDGE('',*,*,#3193,.T.);
#4079=ORIENTED_EDGE('',*,*,#3178,.F.);
#4080=ORIENTED_EDGE('',*,*,#3193,.F.);
#4081=ORIENTED_EDGE('',*,*,#3194,.F.);
#4082=ORIENTED_EDGE('',*,*,#3147,.T.);
#4083=ORIENTED_EDGE('',*,*,#3195,.T.);
#4084=ORIENTED_EDGE('',*,*,#3179,.F.);
#4085=ORIENTED_EDGE('',*,*,#3195,.F.);
#4086=ORIENTED_EDGE('',*,*,#3146,.T.);
#4087=ORIENTED_EDGE('',*,*,#3196,.T.);
#4088=ORIENTED_EDGE('',*,*,#3181,.F.);
#4089=ORIENTED_EDGE('',*,*,#3196,.F.);
#4090=ORIENTED_EDGE('',*,*,#3145,.T.);
#4091=ORIENTED_EDGE('',*,*,#3197,.T.);
#4092=ORIENTED_EDGE('',*,*,#3183,.F.);
#4093=ORIENTED_EDGE('',*,*,#3197,.F.);
#4094=ORIENTED_EDGE('',*,*,#3144,.T.);
#4095=ORIENTED_EDGE('',*,*,#3198,.T.);
#4096=ORIENTED_EDGE('',*,*,#3185,.F.);
#4097=ORIENTED_EDGE('',*,*,#3198,.F.);
#4098=ORIENTED_EDGE('',*,*,#3151,.T.);
#4099=ORIENTED_EDGE('',*,*,#3199,.T.);
#4100=ORIENTED_EDGE('',*,*,#3187,.F.);
#4101=ORIENTED_EDGE('',*,*,#3199,.F.);
#4102=ORIENTED_EDGE('',*,*,#3150,.T.);
#4103=ORIENTED_EDGE('',*,*,#3200,.T.);
#4104=ORIENTED_EDGE('',*,*,#3189,.F.);
#4105=ORIENTED_EDGE('',*,*,#3200,.F.);
#4106=ORIENTED_EDGE('',*,*,#3149,.T.);
#4107=ORIENTED_EDGE('',*,*,#3201,.T.);
#4108=ORIENTED_EDGE('',*,*,#3191,.F.);
#4109=ORIENTED_EDGE('',*,*,#3201,.F.);
#4110=ORIENTED_EDGE('',*,*,#3148,.T.);
#4111=ORIENTED_EDGE('',*,*,#3194,.T.);
#4112=ORIENTED_EDGE('',*,*,#3202,.F.);
#4113=ORIENTED_EDGE('',*,*,#3203,.T.);
#4114=ORIENTED_EDGE('',*,*,#3204,.T.);
#4115=ORIENTED_EDGE('',*,*,#3203,.F.);
#4116=ORIENTED_EDGE('',*,*,#3204,.F.);
#4117=ORIENTED_EDGE('',*,*,#3205,.F.);
#4118=ORIENTED_EDGE('',*,*,#3206,.F.);
#4119=ORIENTED_EDGE('',*,*,#3207,.T.);
#4120=ORIENTED_EDGE('',*,*,#3208,.T.);
#4121=ORIENTED_EDGE('',*,*,#3207,.F.);
#4122=ORIENTED_EDGE('',*,*,#3208,.F.);
#4123=ORIENTED_EDGE('',*,*,#3209,.F.);
#4124=ORIENTED_EDGE('',*,*,#3210,.T.);
#4125=ORIENTED_EDGE('',*,*,#3211,.T.);
#4126=ORIENTED_EDGE('',*,*,#3212,.T.);
#4127=ORIENTED_EDGE('',*,*,#3213,.T.);
#4128=ORIENTED_EDGE('',*,*,#3214,.T.);
#4129=ORIENTED_EDGE('',*,*,#3215,.T.);
#4130=ORIENTED_EDGE('',*,*,#3216,.T.);
#4131=ORIENTED_EDGE('',*,*,#3216,.F.);
#4132=ORIENTED_EDGE('',*,*,#3217,.T.);
#4133=ORIENTED_EDGE('',*,*,#3218,.F.);
#4134=ORIENTED_EDGE('',*,*,#3219,.F.);
#4135=ORIENTED_EDGE('',*,*,#3217,.F.);
#4136=ORIENTED_EDGE('',*,*,#3218,.T.);
#4137=ORIENTED_EDGE('',*,*,#3219,.T.);
#4138=ORIENTED_EDGE('',*,*,#3220,.T.);
#4139=ORIENTED_EDGE('',*,*,#3221,.F.);
#4140=ORIENTED_EDGE('',*,*,#3220,.F.);
#4141=ORIENTED_EDGE('',*,*,#3221,.T.);
#4142=ORIENTED_EDGE('',*,*,#3222,.T.);
#4143=ORIENTED_EDGE('',*,*,#3222,.F.);
#4144=ORIENTED_EDGE('',*,*,#3223,.T.);
#4145=ORIENTED_EDGE('',*,*,#3224,.T.);
#4146=ORIENTED_EDGE('',*,*,#3223,.F.);
#4147=ORIENTED_EDGE('',*,*,#3225,.T.);
#4148=ORIENTED_EDGE('',*,*,#3226,.T.);
#4149=ORIENTED_EDGE('',*,*,#3227,.T.);
#4150=ORIENTED_EDGE('',*,*,#3224,.F.);
#4151=ORIENTED_EDGE('',*,*,#3227,.F.);
#4152=ORIENTED_EDGE('',*,*,#3228,.T.);
#4153=ORIENTED_EDGE('',*,*,#3229,.T.);
#4154=ORIENTED_EDGE('',*,*,#3230,.T.);
#4155=ORIENTED_EDGE('',*,*,#3228,.F.);
#4156=ORIENTED_EDGE('',*,*,#3229,.F.);
#4157=ORIENTED_EDGE('',*,*,#3230,.F.);
#4158=ORIENTED_EDGE('',*,*,#3231,.T.);
#4159=ORIENTED_EDGE('',*,*,#3232,.T.);
#4160=ORIENTED_EDGE('',*,*,#3231,.F.);
#4161=ORIENTED_EDGE('',*,*,#3233,.T.);
#4162=ORIENTED_EDGE('',*,*,#3234,.T.);
#4163=ORIENTED_EDGE('',*,*,#3235,.T.);
#4164=ORIENTED_EDGE('',*,*,#3236,.T.);
#4165=ORIENTED_EDGE('',*,*,#3237,.T.);
#4166=ORIENTED_EDGE('',*,*,#3238,.T.);
#4167=ORIENTED_EDGE('',*,*,#3232,.F.);
#4168=ORIENTED_EDGE('',*,*,#3239,.T.);
#4169=ORIENTED_EDGE('',*,*,#3240,.F.);
#4170=ORIENTED_EDGE('',*,*,#3233,.F.);
#4171=ORIENTED_EDGE('',*,*,#3241,.F.);
#4172=ORIENTED_EDGE('',*,*,#3242,.T.);
#4173=ORIENTED_EDGE('',*,*,#3243,.F.);
#4174=ORIENTED_EDGE('',*,*,#3244,.F.);
#4175=ORIENTED_EDGE('',*,*,#3239,.F.);
#4176=ORIENTED_EDGE('',*,*,#3242,.F.);
#4177=ORIENTED_EDGE('',*,*,#3245,.F.);
#4178=ORIENTED_EDGE('',*,*,#3246,.T.);
#4179=ORIENTED_EDGE('',*,*,#3247,.F.);
#4180=ORIENTED_EDGE('',*,*,#3248,.T.);
#4181=ORIENTED_EDGE('',*,*,#3249,.T.);
#4182=ORIENTED_EDGE('',*,*,#3247,.T.);
#4183=ORIENTED_EDGE('',*,*,#3212,.F.);
#4184=ORIENTED_EDGE('',*,*,#3248,.F.);
#4185=ORIENTED_EDGE('',*,*,#3250,.T.);
#4186=ORIENTED_EDGE('',*,*,#3251,.F.);
#4187=ORIENTED_EDGE('',*,*,#3213,.F.);
#4188=ORIENTED_EDGE('',*,*,#3251,.T.);
#4189=ORIENTED_EDGE('',*,*,#3252,.T.);
#4190=ORIENTED_EDGE('',*,*,#3253,.F.);
#4191=ORIENTED_EDGE('',*,*,#3254,.T.);
#4192=ORIENTED_EDGE('',*,*,#3255,.F.);
#4193=ORIENTED_EDGE('',*,*,#3214,.F.);
#4194=ORIENTED_EDGE('',*,*,#3253,.T.);
#4195=ORIENTED_EDGE('',*,*,#3246,.F.);
#4196=ORIENTED_EDGE('',*,*,#3256,.F.);
#4197=ORIENTED_EDGE('',*,*,#3257,.F.);
#4198=ORIENTED_EDGE('',*,*,#3258,.F.);
#4199=ORIENTED_EDGE('',*,*,#3250,.F.);
#4200=ORIENTED_EDGE('',*,*,#3254,.F.);
#4201=ORIENTED_EDGE('',*,*,#3259,.F.);
#4202=ORIENTED_EDGE('',*,*,#3260,.F.);
#4203=ORIENTED_EDGE('',*,*,#3261,.T.);
#4204=ORIENTED_EDGE('',*,*,#3259,.T.);
#4205=ORIENTED_EDGE('',*,*,#3252,.F.);
#4206=ORIENTED_EDGE('',*,*,#3258,.T.);
#4207=ORIENTED_EDGE('',*,*,#3262,.T.);
#4208=ORIENTED_EDGE('',*,*,#3263,.F.);
#4209=ORIENTED_EDGE('',*,*,#3264,.F.);
#4210=ORIENTED_EDGE('',*,*,#3262,.F.);
#4211=ORIENTED_EDGE('',*,*,#3257,.T.);
#4212=ORIENTED_EDGE('',*,*,#3265,.F.);
#4213=ORIENTED_EDGE('',*,*,#3237,.F.);
#4214=ORIENTED_EDGE('',*,*,#3266,.T.);
#4215=ORIENTED_EDGE('',*,*,#3265,.T.);
#4216=ORIENTED_EDGE('',*,*,#3267,.F.);
#4217=ORIENTED_EDGE('',*,*,#3256,.T.);
#4218=ORIENTED_EDGE('',*,*,#3268,.F.);
#4219=ORIENTED_EDGE('',*,*,#3238,.F.);
#4220=ORIENTED_EDGE('',*,*,#3267,.T.);
#4221=ORIENTED_EDGE('',*,*,#3268,.T.);
#4222=ORIENTED_EDGE('',*,*,#3245,.T.);
#4223=ORIENTED_EDGE('',*,*,#3241,.T.);
#4224=ORIENTED_EDGE('',*,*,#3236,.F.);
#4225=ORIENTED_EDGE('',*,*,#3269,.F.);
#4226=ORIENTED_EDGE('',*,*,#3260,.T.);
#4227=ORIENTED_EDGE('',*,*,#3266,.F.);
#4228=ORIENTED_EDGE('',*,*,#3269,.T.);
#4229=ORIENTED_EDGE('',*,*,#3270,.T.);
#4230=ORIENTED_EDGE('',*,*,#3271,.T.);
#4231=ORIENTED_EDGE('',*,*,#3261,.F.);
#4232=ORIENTED_EDGE('',*,*,#3271,.F.);
#4233=ORIENTED_EDGE('',*,*,#3272,.T.);
#4234=ORIENTED_EDGE('',*,*,#3273,.F.);
#4235=ORIENTED_EDGE('',*,*,#3274,.T.);
#4236=ORIENTED_EDGE('',*,*,#3255,.T.);
#4237=ORIENTED_EDGE('',*,*,#3273,.T.);
#4238=ORIENTED_EDGE('',*,*,#3275,.T.);
#4239=ORIENTED_EDGE('',*,*,#3276,.F.);
#4240=ORIENTED_EDGE('',*,*,#3215,.F.);
#4241=ORIENTED_EDGE('',*,*,#3274,.F.);
#4242=ORIENTED_EDGE('',*,*,#3272,.F.);
#4243=ORIENTED_EDGE('',*,*,#3277,.F.);
#4244=ORIENTED_EDGE('',*,*,#3278,.T.);
#4245=ORIENTED_EDGE('',*,*,#3275,.F.);
#4246=ORIENTED_EDGE('',*,*,#3278,.F.);
#4247=ORIENTED_EDGE('',*,*,#3279,.F.);
#4248=ORIENTED_EDGE('',*,*,#3280,.T.);
#4249=ORIENTED_EDGE('',*,*,#3281,.F.);
#4250=ORIENTED_EDGE('',*,*,#3281,.T.);
#4251=ORIENTED_EDGE('',*,*,#3282,.T.);
#4252=ORIENTED_EDGE('',*,*,#3276,.T.);
#4253=ORIENTED_EDGE('',*,*,#3210,.F.);
#4254=ORIENTED_EDGE('',*,*,#3282,.F.);
#4255=ORIENTED_EDGE('',*,*,#3283,.T.);
#4256=ORIENTED_EDGE('',*,*,#3284,.F.);
#4257=ORIENTED_EDGE('',*,*,#3285,.T.);
#4258=ORIENTED_EDGE('',*,*,#3284,.T.);
#4259=ORIENTED_EDGE('',*,*,#3286,.T.);
#4260=ORIENTED_EDGE('',*,*,#3211,.F.);
#4261=ORIENTED_EDGE('',*,*,#3285,.F.);
#4262=ORIENTED_EDGE('',*,*,#3243,.T.);
#4263=ORIENTED_EDGE('',*,*,#3249,.F.);
#4264=ORIENTED_EDGE('',*,*,#3287,.F.);
#4265=ORIENTED_EDGE('',*,*,#3288,.F.);
#4266=ORIENTED_EDGE('',*,*,#3244,.T.);
#4267=ORIENTED_EDGE('',*,*,#3286,.F.);
#4268=ORIENTED_EDGE('',*,*,#3289,.F.);
#4269=ORIENTED_EDGE('',*,*,#3287,.T.);
#4270=ORIENTED_EDGE('',*,*,#3283,.F.);
#4271=ORIENTED_EDGE('',*,*,#3280,.F.);
#4272=ORIENTED_EDGE('',*,*,#3290,.F.);
#4273=ORIENTED_EDGE('',*,*,#3289,.T.);
#4274=ORIENTED_EDGE('',*,*,#3291,.F.);
#4275=ORIENTED_EDGE('',*,*,#3234,.F.);
#4276=ORIENTED_EDGE('',*,*,#3292,.F.);
#4277=ORIENTED_EDGE('',*,*,#3288,.T.);
#4278=ORIENTED_EDGE('',*,*,#3292,.T.);
#4279=ORIENTED_EDGE('',*,*,#3240,.T.);
#4280=ORIENTED_EDGE('',*,*,#3293,.T.);
#4281=ORIENTED_EDGE('',*,*,#3291,.T.);
#4282=ORIENTED_EDGE('',*,*,#3279,.T.);
#4283=ORIENTED_EDGE('',*,*,#3235,.F.);
#4284=ORIENTED_EDGE('',*,*,#3293,.F.);
#4285=ORIENTED_EDGE('',*,*,#3277,.T.);
#4286=ORIENTED_EDGE('',*,*,#3270,.F.);
#4287=ORIENTED_EDGE('',*,*,#3294,.F.);
#4288=ORIENTED_EDGE('',*,*,#3295,.T.);
#4289=ORIENTED_EDGE('',*,*,#3290,.T.);
#4290=ORIENTED_EDGE('',*,*,#3295,.F.);
#4291=ORIENTED_EDGE('',*,*,#3294,.T.);
#4292=ORIENTED_EDGE('',*,*,#3296,.F.);
#4293=ORIENTED_EDGE('',*,*,#3297,.F.);
#4294=ORIENTED_EDGE('',*,*,#3298,.T.);
#4295=ORIENTED_EDGE('',*,*,#3296,.T.);
#4296=ORIENTED_EDGE('',*,*,#3298,.F.);
#4297=ORIENTED_EDGE('',*,*,#3225,.F.);
#4298=ORIENTED_EDGE('',*,*,#3226,.F.);
#4299=ORIENTED_EDGE('',*,*,#3299,.T.);
#4300=ORIENTED_EDGE('',*,*,#3297,.T.);
#4301=ORIENTED_EDGE('',*,*,#3299,.F.);
#4302=ORIENTED_EDGE('',*,*,#3300,.T.);
#4303=ORIENTED_EDGE('',*,*,#3301,.T.);
#4304=ORIENTED_EDGE('',*,*,#3263,.T.);
#4305=ORIENTED_EDGE('',*,*,#3264,.T.);
#4306=ORIENTED_EDGE('',*,*,#3301,.F.);
#4307=ORIENTED_EDGE('',*,*,#3302,.T.);
#4308=ORIENTED_EDGE('',*,*,#3303,.T.);
#4309=ORIENTED_EDGE('',*,*,#3304,.T.);
#4310=ORIENTED_EDGE('',*,*,#3305,.T.);
#4311=ORIENTED_EDGE('',*,*,#3306,.F.);
#4312=ORIENTED_EDGE('',*,*,#3307,.F.);
#4313=ORIENTED_EDGE('',*,*,#3305,.F.);
#4314=ORIENTED_EDGE('',*,*,#3300,.F.);
#4315=ORIENTED_EDGE('',*,*,#3308,.T.);
#4316=ORIENTED_EDGE('',*,*,#3306,.T.);
#4317=ORIENTED_EDGE('',*,*,#3307,.T.);
#4318=ORIENTED_EDGE('',*,*,#3308,.F.);
#4319=ORIENTED_EDGE('',*,*,#3302,.F.);
#4320=ORIENTED_EDGE('',*,*,#3303,.F.);
#4321=ORIENTED_EDGE('',*,*,#3304,.F.);
#4322=ORIENTED_EDGE('',*,*,#3309,.T.);
#4323=ORIENTED_EDGE('',*,*,#3310,.F.);
#4324=ORIENTED_EDGE('',*,*,#3311,.T.);
#4325=ORIENTED_EDGE('',*,*,#3312,.T.);
#4326=ORIENTED_EDGE('',*,*,#3313,.T.);
#4327=ORIENTED_EDGE('',*,*,#3314,.T.);
#4328=ORIENTED_EDGE('',*,*,#3315,.T.);
#4329=ORIENTED_EDGE('',*,*,#3316,.T.);
#4330=ORIENTED_EDGE('',*,*,#3317,.F.);
#4331=ORIENTED_EDGE('',*,*,#3318,.T.);
#4332=ORIENTED_EDGE('',*,*,#3319,.F.);
#4333=ORIENTED_EDGE('',*,*,#3309,.F.);
#4334=ORIENTED_EDGE('',*,*,#3320,.F.);
#4335=ORIENTED_EDGE('',*,*,#3321,.T.);
#4336=ORIENTED_EDGE('',*,*,#3317,.T.);
#4337=ORIENTED_EDGE('',*,*,#3322,.F.);
#4338=ORIENTED_EDGE('',*,*,#3323,.T.);
#4339=ORIENTED_EDGE('',*,*,#3320,.T.);
#4340=ORIENTED_EDGE('',*,*,#3324,.T.);
#4341=ORIENTED_EDGE('',*,*,#3325,.F.);
#4342=ORIENTED_EDGE('',*,*,#3326,.T.);
#4343=ORIENTED_EDGE('',*,*,#3327,.T.);
#4344=ORIENTED_EDGE('',*,*,#3328,.F.);
#4345=ORIENTED_EDGE('',*,*,#3329,.T.);
#4346=ORIENTED_EDGE('',*,*,#3330,.T.);
#4347=ORIENTED_EDGE('',*,*,#3331,.F.);
#4348=ORIENTED_EDGE('',*,*,#3332,.F.);
#4349=ORIENTED_EDGE('',*,*,#3333,.T.);
#4350=ORIENTED_EDGE('',*,*,#3333,.F.);
#4351=ORIENTED_EDGE('',*,*,#3334,.T.);
#4352=ORIENTED_EDGE('',*,*,#3335,.F.);
#4353=ORIENTED_EDGE('',*,*,#3336,.F.);
#4354=ORIENTED_EDGE('',*,*,#3337,.T.);
#4355=ORIENTED_EDGE('',*,*,#3338,.T.);
#4356=ORIENTED_EDGE('',*,*,#3337,.F.);
#4357=ORIENTED_EDGE('',*,*,#3339,.F.);
#4358=ORIENTED_EDGE('',*,*,#3334,.F.);
#4359=ORIENTED_EDGE('',*,*,#3338,.F.);
#4360=ORIENTED_EDGE('',*,*,#3336,.T.);
#4361=ORIENTED_EDGE('',*,*,#3340,.T.);
#4362=ORIENTED_EDGE('',*,*,#3341,.T.);
#4363=ORIENTED_EDGE('',*,*,#3340,.F.);
#4364=ORIENTED_EDGE('',*,*,#3335,.T.);
#4365=ORIENTED_EDGE('',*,*,#3339,.T.);
#4366=ORIENTED_EDGE('',*,*,#3342,.T.);
#4367=ORIENTED_EDGE('',*,*,#3332,.T.);
#4368=ORIENTED_EDGE('',*,*,#3343,.T.);
#4369=ORIENTED_EDGE('',*,*,#3344,.T.);
#4370=ORIENTED_EDGE('',*,*,#3345,.T.);
#4371=ORIENTED_EDGE('',*,*,#3346,.T.);
#4372=ORIENTED_EDGE('',*,*,#3310,.T.);
#4373=ORIENTED_EDGE('',*,*,#3319,.T.);
#4374=ORIENTED_EDGE('',*,*,#3347,.T.);
#4375=ORIENTED_EDGE('',*,*,#3348,.T.);
#4376=ORIENTED_EDGE('',*,*,#3349,.T.);
#4377=ORIENTED_EDGE('',*,*,#3350,.F.);
#4378=ORIENTED_EDGE('',*,*,#3328,.T.);
#4379=ORIENTED_EDGE('',*,*,#3351,.F.);
#4380=ORIENTED_EDGE('',*,*,#3352,.T.);
#4381=ORIENTED_EDGE('',*,*,#3353,.T.);
#4382=ORIENTED_EDGE('',*,*,#3354,.T.);
#4383=ORIENTED_EDGE('',*,*,#3355,.T.);
#4384=ORIENTED_EDGE('',*,*,#3356,.T.);
#4385=ORIENTED_EDGE('',*,*,#3357,.F.);
#4386=ORIENTED_EDGE('',*,*,#3358,.F.);
#4387=ORIENTED_EDGE('',*,*,#3341,.F.);
#4388=ORIENTED_EDGE('',*,*,#3359,.T.);
#4389=ORIENTED_EDGE('',*,*,#3360,.T.);
#4390=ORIENTED_EDGE('',*,*,#3358,.T.);
#4391=ORIENTED_EDGE('',*,*,#3360,.F.);
#4392=ORIENTED_EDGE('',*,*,#3361,.T.);
#4393=ORIENTED_EDGE('',*,*,#3362,.T.);
#4394=ORIENTED_EDGE('',*,*,#3363,.T.);
#4395=ORIENTED_EDGE('',*,*,#3364,.F.);
#4396=ORIENTED_EDGE('',*,*,#3365,.T.);
#4397=ORIENTED_EDGE('',*,*,#3361,.F.);
#4398=ORIENTED_EDGE('',*,*,#3359,.F.);
#4399=ORIENTED_EDGE('',*,*,#3363,.F.);
#4400=ORIENTED_EDGE('',*,*,#3366,.T.);
#4401=ORIENTED_EDGE('',*,*,#3367,.T.);
#4402=ORIENTED_EDGE('',*,*,#3366,.F.);
#4403=ORIENTED_EDGE('',*,*,#3362,.F.);
#4404=ORIENTED_EDGE('',*,*,#3365,.F.);
#4405=ORIENTED_EDGE('',*,*,#3368,.F.);
#4406=ORIENTED_EDGE('',*,*,#3369,.F.);
#4407=ORIENTED_EDGE('',*,*,#3370,.F.);
#4408=ORIENTED_EDGE('',*,*,#3371,.F.);
#4409=ORIENTED_EDGE('',*,*,#3372,.F.);
#4410=ORIENTED_EDGE('',*,*,#3373,.F.);
#4411=ORIENTED_EDGE('',*,*,#3344,.F.);
#4412=ORIENTED_EDGE('',*,*,#3374,.T.);
#4413=ORIENTED_EDGE('',*,*,#3375,.F.);
#4414=ORIENTED_EDGE('',*,*,#3376,.F.);
#4415=ORIENTED_EDGE('',*,*,#3349,.F.);
#4416=ORIENTED_EDGE('',*,*,#3377,.T.);
#4417=ORIENTED_EDGE('',*,*,#3367,.F.);
#4418=ORIENTED_EDGE('',*,*,#3364,.T.);
#4419=ORIENTED_EDGE('',*,*,#3368,.T.);
#4420=ORIENTED_EDGE('',*,*,#3378,.F.);
#4421=ORIENTED_EDGE('',*,*,#3379,.F.);
#4422=ORIENTED_EDGE('',*,*,#3380,.F.);
#4423=ORIENTED_EDGE('',*,*,#3381,.F.);
#4424=ORIENTED_EDGE('',*,*,#3382,.F.);
#4425=ORIENTED_EDGE('',*,*,#3383,.T.);
#4426=ORIENTED_EDGE('',*,*,#3381,.T.);
#4427=ORIENTED_EDGE('',*,*,#3384,.T.);
#4428=ORIENTED_EDGE('',*,*,#3385,.T.);
#4429=ORIENTED_EDGE('',*,*,#3386,.F.);
#4430=ORIENTED_EDGE('',*,*,#3315,.F.);
#4431=ORIENTED_EDGE('',*,*,#3387,.F.);
#4432=ORIENTED_EDGE('',*,*,#3388,.T.);
#4433=ORIENTED_EDGE('',*,*,#3382,.T.);
#4434=ORIENTED_EDGE('',*,*,#3389,.T.);
#4435=ORIENTED_EDGE('',*,*,#3390,.T.);
#4436=ORIENTED_EDGE('',*,*,#3391,.F.);
#4437=ORIENTED_EDGE('',*,*,#3392,.T.);
#4438=ORIENTED_EDGE('',*,*,#3393,.T.);
#4439=ORIENTED_EDGE('',*,*,#3394,.T.);
#4440=ORIENTED_EDGE('',*,*,#3395,.F.);
#4441=ORIENTED_EDGE('',*,*,#3395,.T.);
#4442=ORIENTED_EDGE('',*,*,#3396,.T.);
#4443=ORIENTED_EDGE('',*,*,#3348,.F.);
#4444=ORIENTED_EDGE('',*,*,#3396,.F.);
#4445=ORIENTED_EDGE('',*,*,#3385,.F.);
#4446=ORIENTED_EDGE('',*,*,#3397,.F.);
#4447=ORIENTED_EDGE('',*,*,#3325,.T.);
#4448=ORIENTED_EDGE('',*,*,#3398,.T.);
#4449=ORIENTED_EDGE('',*,*,#3399,.T.);
#4450=ORIENTED_EDGE('',*,*,#3398,.F.);
#4451=ORIENTED_EDGE('',*,*,#3324,.F.);
#4452=ORIENTED_EDGE('',*,*,#3322,.T.);
#4453=ORIENTED_EDGE('',*,*,#3400,.F.);
#4454=ORIENTED_EDGE('',*,*,#3347,.F.);
#4455=ORIENTED_EDGE('',*,*,#3318,.F.);
#4456=ORIENTED_EDGE('',*,*,#3399,.F.);
#4457=ORIENTED_EDGE('',*,*,#3316,.F.);
#4458=ORIENTED_EDGE('',*,*,#3386,.T.);
#4459=ORIENTED_EDGE('',*,*,#3401,.T.);
#4460=ORIENTED_EDGE('',*,*,#3311,.F.);
#4461=ORIENTED_EDGE('',*,*,#3346,.F.);
#4462=ORIENTED_EDGE('',*,*,#3402,.T.);
#4463=ORIENTED_EDGE('',*,*,#3387,.T.);
#4464=ORIENTED_EDGE('',*,*,#3314,.F.);
#4465=ORIENTED_EDGE('',*,*,#3342,.F.);
#4466=ORIENTED_EDGE('',*,*,#3400,.T.);
#4467=ORIENTED_EDGE('',*,*,#3321,.F.);
#4468=ORIENTED_EDGE('',*,*,#3323,.F.);
#4469=ORIENTED_EDGE('',*,*,#3345,.F.);
#4470=ORIENTED_EDGE('',*,*,#3373,.T.);
#4471=ORIENTED_EDGE('',*,*,#3403,.F.);
#4472=ORIENTED_EDGE('',*,*,#3401,.F.);
#4473=ORIENTED_EDGE('',*,*,#3312,.F.);
#4474=ORIENTED_EDGE('',*,*,#3403,.T.);
#4475=ORIENTED_EDGE('',*,*,#3372,.T.);
#4476=ORIENTED_EDGE('',*,*,#3404,.F.);
#4477=ORIENTED_EDGE('',*,*,#3313,.F.);
#4478=ORIENTED_EDGE('',*,*,#3404,.T.);
#4479=ORIENTED_EDGE('',*,*,#3371,.T.);
#4480=ORIENTED_EDGE('',*,*,#3405,.F.);
#4481=ORIENTED_EDGE('',*,*,#3370,.T.);
#4482=ORIENTED_EDGE('',*,*,#3406,.T.);
#4483=ORIENTED_EDGE('',*,*,#3402,.F.);
#4484=ORIENTED_EDGE('',*,*,#3405,.T.);
#4485=ORIENTED_EDGE('',*,*,#3388,.F.);
#4486=ORIENTED_EDGE('',*,*,#3406,.F.);
#4487=ORIENTED_EDGE('',*,*,#3369,.T.);
#4488=ORIENTED_EDGE('',*,*,#3383,.F.);
#4489=ORIENTED_EDGE('',*,*,#3394,.F.);
#4490=ORIENTED_EDGE('',*,*,#3407,.T.);
#4491=ORIENTED_EDGE('',*,*,#3408,.T.);
#4492=ORIENTED_EDGE('',*,*,#3397,.T.);
#4493=ORIENTED_EDGE('',*,*,#3409,.T.);
#4494=ORIENTED_EDGE('',*,*,#3410,.T.);
#4495=ORIENTED_EDGE('',*,*,#3411,.F.);
#4496=ORIENTED_EDGE('',*,*,#3326,.F.);
#4497=ORIENTED_EDGE('',*,*,#3408,.F.);
#4498=ORIENTED_EDGE('',*,*,#3412,.F.);
#4499=ORIENTED_EDGE('',*,*,#3409,.F.);
#4500=ORIENTED_EDGE('',*,*,#3413,.F.);
#4501=ORIENTED_EDGE('',*,*,#3414,.F.);
#4502=ORIENTED_EDGE('',*,*,#3415,.F.);
#4503=ORIENTED_EDGE('',*,*,#3410,.F.);
#4504=ORIENTED_EDGE('',*,*,#3416,.F.);
#4505=ORIENTED_EDGE('',*,*,#3417,.F.);
#4506=ORIENTED_EDGE('',*,*,#3418,.T.);
#4507=ORIENTED_EDGE('',*,*,#3416,.T.);
#4508=ORIENTED_EDGE('',*,*,#3412,.T.);
#4509=ORIENTED_EDGE('',*,*,#3418,.F.);
#4510=ORIENTED_EDGE('',*,*,#3419,.T.);
#4511=ORIENTED_EDGE('',*,*,#3420,.F.);
#4512=ORIENTED_EDGE('',*,*,#3421,.T.);
#4513=ORIENTED_EDGE('',*,*,#3391,.T.);
#4514=ORIENTED_EDGE('',*,*,#3422,.T.);
#4515=ORIENTED_EDGE('',*,*,#3423,.T.);
#4516=ORIENTED_EDGE('',*,*,#3424,.T.);
#4517=ORIENTED_EDGE('',*,*,#3354,.F.);
#4518=ORIENTED_EDGE('',*,*,#3417,.T.);
#4519=ORIENTED_EDGE('',*,*,#3425,.T.);
#4520=ORIENTED_EDGE('',*,*,#3425,.F.);
#4521=ORIENTED_EDGE('',*,*,#3426,.T.);
#4522=ORIENTED_EDGE('',*,*,#3427,.T.);
#4523=ORIENTED_EDGE('',*,*,#3426,.F.);
#4524=ORIENTED_EDGE('',*,*,#3427,.F.);
#4525=ORIENTED_EDGE('',*,*,#3379,.T.);
#4526=ORIENTED_EDGE('',*,*,#3428,.F.);
#4527=ORIENTED_EDGE('',*,*,#3429,.T.);
#4528=ORIENTED_EDGE('',*,*,#3430,.F.);
#4529=ORIENTED_EDGE('',*,*,#3380,.T.);
#4530=ORIENTED_EDGE('',*,*,#3389,.F.);
#4531=ORIENTED_EDGE('',*,*,#3384,.F.);
#4532=ORIENTED_EDGE('',*,*,#3430,.T.);
#4533=ORIENTED_EDGE('',*,*,#3431,.F.);
#4534=ORIENTED_EDGE('',*,*,#3432,.T.);
#4535=ORIENTED_EDGE('',*,*,#3431,.T.);
#4536=ORIENTED_EDGE('',*,*,#3433,.T.);
#4537=ORIENTED_EDGE('',*,*,#3422,.F.);
#4538=ORIENTED_EDGE('',*,*,#3390,.F.);
#4539=ORIENTED_EDGE('',*,*,#3432,.F.);
#4540=ORIENTED_EDGE('',*,*,#3434,.T.);
#4541=ORIENTED_EDGE('',*,*,#3435,.F.);
#4542=ORIENTED_EDGE('',*,*,#3423,.F.);
#4543=ORIENTED_EDGE('',*,*,#3434,.F.);
#4544=ORIENTED_EDGE('',*,*,#3436,.F.);
#4545=ORIENTED_EDGE('',*,*,#3424,.F.);
#4546=ORIENTED_EDGE('',*,*,#3435,.T.);
#4547=ORIENTED_EDGE('',*,*,#3437,.F.);
#4548=ORIENTED_EDGE('',*,*,#3355,.F.);
#4549=ORIENTED_EDGE('',*,*,#3438,.T.);
#4550=ORIENTED_EDGE('',*,*,#3437,.T.);
#4551=ORIENTED_EDGE('',*,*,#3439,.T.);
#4552=ORIENTED_EDGE('',*,*,#3428,.T.);
#4553=ORIENTED_EDGE('',*,*,#3440,.F.);
#4554=ORIENTED_EDGE('',*,*,#3356,.F.);
#4555=ORIENTED_EDGE('',*,*,#3438,.F.);
#4556=ORIENTED_EDGE('',*,*,#3377,.F.);
#4557=ORIENTED_EDGE('',*,*,#3357,.T.);
#4558=ORIENTED_EDGE('',*,*,#3440,.T.);
#4559=ORIENTED_EDGE('',*,*,#3378,.T.);
#4560=ORIENTED_EDGE('',*,*,#3429,.F.);
#4561=ORIENTED_EDGE('',*,*,#3439,.F.);
#4562=ORIENTED_EDGE('',*,*,#3436,.T.);
#4563=ORIENTED_EDGE('',*,*,#3433,.F.);
#4564=ORIENTED_EDGE('',*,*,#3419,.F.);
#4565=ORIENTED_EDGE('',*,*,#3353,.F.);
#4566=ORIENTED_EDGE('',*,*,#3441,.F.);
#4567=ORIENTED_EDGE('',*,*,#3442,.T.);
#4568=ORIENTED_EDGE('',*,*,#3442,.F.);
#4569=ORIENTED_EDGE('',*,*,#3443,.T.);
#4570=ORIENTED_EDGE('',*,*,#3444,.F.);
#4571=ORIENTED_EDGE('',*,*,#3420,.T.);
#4572=ORIENTED_EDGE('',*,*,#3421,.F.);
#4573=ORIENTED_EDGE('',*,*,#3444,.T.);
#4574=ORIENTED_EDGE('',*,*,#3445,.F.);
#4575=ORIENTED_EDGE('',*,*,#3392,.F.);
#4576=ORIENTED_EDGE('',*,*,#3445,.T.);
#4577=ORIENTED_EDGE('',*,*,#3446,.T.);
#4578=ORIENTED_EDGE('',*,*,#3447,.T.);
#4579=ORIENTED_EDGE('',*,*,#3393,.F.);
#4580=ORIENTED_EDGE('',*,*,#3447,.F.);
#4581=ORIENTED_EDGE('',*,*,#3413,.T.);
#4582=ORIENTED_EDGE('',*,*,#3407,.F.);
#4583=ORIENTED_EDGE('',*,*,#3443,.F.);
#4584=ORIENTED_EDGE('',*,*,#3448,.F.);
#4585=ORIENTED_EDGE('',*,*,#3414,.T.);
#4586=ORIENTED_EDGE('',*,*,#3446,.F.);
#4587=ORIENTED_EDGE('',*,*,#3448,.T.);
#4588=ORIENTED_EDGE('',*,*,#3441,.T.);
#4589=ORIENTED_EDGE('',*,*,#3449,.T.);
#4590=ORIENTED_EDGE('',*,*,#3415,.T.);
#4591=ORIENTED_EDGE('',*,*,#3449,.F.);
#4592=ORIENTED_EDGE('',*,*,#3352,.F.);
#4593=ORIENTED_EDGE('',*,*,#3450,.F.);
#4594=ORIENTED_EDGE('',*,*,#3327,.F.);
#4595=ORIENTED_EDGE('',*,*,#3411,.T.);
#4596=ORIENTED_EDGE('',*,*,#3450,.T.);
#4597=ORIENTED_EDGE('',*,*,#3351,.T.);
#4598=ORIENTED_EDGE('',*,*,#3350,.T.);
#4599=ORIENTED_EDGE('',*,*,#3376,.T.);
#4600=ORIENTED_EDGE('',*,*,#3451,.F.);
#4601=ORIENTED_EDGE('',*,*,#3329,.F.);
#4602=ORIENTED_EDGE('',*,*,#3375,.T.);
#4603=ORIENTED_EDGE('',*,*,#3452,.F.);
#4604=ORIENTED_EDGE('',*,*,#3330,.F.);
#4605=ORIENTED_EDGE('',*,*,#3451,.T.);
#4606=ORIENTED_EDGE('',*,*,#3343,.F.);
#4607=ORIENTED_EDGE('',*,*,#3331,.T.);
#4608=ORIENTED_EDGE('',*,*,#3452,.T.);
#4609=ORIENTED_EDGE('',*,*,#3374,.F.);
#4610=ORIENTED_EDGE('',*,*,#3453,.F.);
#4611=ORIENTED_EDGE('',*,*,#3454,.T.);
#4612=ORIENTED_EDGE('',*,*,#3455,.T.);
#4613=ORIENTED_EDGE('',*,*,#3454,.F.);
#4614=ORIENTED_EDGE('',*,*,#3455,.F.);
#4615=ORIENTED_EDGE('',*,*,#3456,.F.);
#4616=ORIENTED_EDGE('',*,*,#3457,.F.);
#4617=ORIENTED_EDGE('',*,*,#3458,.T.);
#4618=ORIENTED_EDGE('',*,*,#3459,.T.);
#4619=ORIENTED_EDGE('',*,*,#3458,.F.);
#4620=ORIENTED_EDGE('',*,*,#3459,.F.);
#4621=ORIENTED_EDGE('',*,*,#3460,.F.);
#4622=ORIENTED_EDGE('',*,*,#3461,.F.);
#4623=ORIENTED_EDGE('',*,*,#3462,.F.);
#4624=ORIENTED_EDGE('',*,*,#3463,.F.);
#4625=ORIENTED_EDGE('',*,*,#3464,.F.);
#4626=ORIENTED_EDGE('',*,*,#3465,.F.);
#4627=ORIENTED_EDGE('',*,*,#3466,.F.);
#4628=ORIENTED_EDGE('',*,*,#3467,.T.);
#4629=ORIENTED_EDGE('',*,*,#3461,.T.);
#4630=ORIENTED_EDGE('',*,*,#3468,.T.);
#4631=ORIENTED_EDGE('',*,*,#3469,.F.);
#4632=ORIENTED_EDGE('',*,*,#3470,.F.);
#4633=ORIENTED_EDGE('',*,*,#3462,.T.);
#4634=ORIENTED_EDGE('',*,*,#3470,.T.);
#4635=ORIENTED_EDGE('',*,*,#3471,.F.);
#4636=ORIENTED_EDGE('',*,*,#3472,.F.);
#4637=ORIENTED_EDGE('',*,*,#3463,.T.);
#4638=ORIENTED_EDGE('',*,*,#3472,.T.);
#4639=ORIENTED_EDGE('',*,*,#3473,.F.);
#4640=ORIENTED_EDGE('',*,*,#3474,.F.);
#4641=ORIENTED_EDGE('',*,*,#3464,.T.);
#4642=ORIENTED_EDGE('',*,*,#3474,.T.);
#4643=ORIENTED_EDGE('',*,*,#3475,.F.);
#4644=ORIENTED_EDGE('',*,*,#3476,.F.);
#4645=ORIENTED_EDGE('',*,*,#3465,.T.);
#4646=ORIENTED_EDGE('',*,*,#3476,.T.);
#4647=ORIENTED_EDGE('',*,*,#3477,.F.);
#4648=ORIENTED_EDGE('',*,*,#3478,.F.);
#4649=ORIENTED_EDGE('',*,*,#3466,.T.);
#4650=ORIENTED_EDGE('',*,*,#3478,.T.);
#4651=ORIENTED_EDGE('',*,*,#3479,.F.);
#4652=ORIENTED_EDGE('',*,*,#3468,.F.);
#4653=ORIENTED_EDGE('',*,*,#3469,.T.);
#4654=ORIENTED_EDGE('',*,*,#3479,.T.);
#4655=ORIENTED_EDGE('',*,*,#3477,.T.);
#4656=ORIENTED_EDGE('',*,*,#3475,.T.);
#4657=ORIENTED_EDGE('',*,*,#3473,.T.);
#4658=ORIENTED_EDGE('',*,*,#3471,.T.);
#4659=ORIENTED_EDGE('',*,*,#3480,.F.);
#4660=ORIENTED_EDGE('',*,*,#3467,.F.);
#4661=ORIENTED_EDGE('',*,*,#3481,.T.);
#4662=ORIENTED_EDGE('',*,*,#3482,.T.);
#4663=ORIENTED_EDGE('',*,*,#3481,.F.);
#4664=ORIENTED_EDGE('',*,*,#3483,.F.);
#4665=ORIENTED_EDGE('',*,*,#3484,.T.);
#4666=ORIENTED_EDGE('',*,*,#3480,.T.);
#4667=ORIENTED_EDGE('',*,*,#3484,.F.);
#4668=ORIENTED_EDGE('',*,*,#3482,.F.);
#4669=ORIENTED_EDGE('',*,*,#3485,.T.);
#4670=ORIENTED_EDGE('',*,*,#3485,.F.);
#4671=ORIENTED_EDGE('',*,*,#3486,.T.);
#4672=ORIENTED_EDGE('',*,*,#3487,.T.);
#4673=ORIENTED_EDGE('',*,*,#3486,.F.);
#4674=ORIENTED_EDGE('',*,*,#3483,.T.);
#4675=ORIENTED_EDGE('',*,*,#3487,.F.);
#4676=ORIENTED_EDGE('',*,*,#3488,.F.);
#4677=ORIENTED_EDGE('',*,*,#3489,.T.);
#4678=ORIENTED_EDGE('',*,*,#3490,.T.);
#4679=ORIENTED_EDGE('',*,*,#3489,.F.);
#4680=ORIENTED_EDGE('',*,*,#3491,.F.);
#4681=ORIENTED_EDGE('',*,*,#3490,.F.);
#4682=ORIENTED_EDGE('',*,*,#3492,.F.);
#4683=ORIENTED_EDGE('',*,*,#3493,.T.);
#4684=ORIENTED_EDGE('',*,*,#3494,.T.);
#4685=ORIENTED_EDGE('',*,*,#3493,.F.);
#4686=ORIENTED_EDGE('',*,*,#3495,.F.);
#4687=ORIENTED_EDGE('',*,*,#3494,.F.);
#4688=ORIENTED_EDGE('',*,*,#3496,.T.);
#4689=ORIENTED_EDGE('',*,*,#3497,.T.);
#4690=ORIENTED_EDGE('',*,*,#3496,.F.);
#4691=ORIENTED_EDGE('',*,*,#3498,.T.);
#4692=ORIENTED_EDGE('',*,*,#3499,.T.);
#4693=ORIENTED_EDGE('',*,*,#3498,.F.);
#4694=ORIENTED_EDGE('',*,*,#3500,.T.);
#4695=ORIENTED_EDGE('',*,*,#3501,.T.);
#4696=ORIENTED_EDGE('',*,*,#3502,.T.);
#4697=ORIENTED_EDGE('',*,*,#3503,.T.);
#4698=ORIENTED_EDGE('',*,*,#3499,.F.);
#4699=ORIENTED_EDGE('',*,*,#3504,.T.);
#4700=ORIENTED_EDGE('',*,*,#3505,.T.);
#4701=ORIENTED_EDGE('',*,*,#3506,.T.);
#4702=ORIENTED_EDGE('',*,*,#3507,.T.);
#4703=ORIENTED_EDGE('',*,*,#3508,.T.);
#4704=ORIENTED_EDGE('',*,*,#3509,.T.);
#4705=ORIENTED_EDGE('',*,*,#3510,.T.);
#4706=ORIENTED_EDGE('',*,*,#3511,.T.);
#4707=ORIENTED_EDGE('',*,*,#3503,.F.);
#4708=ORIENTED_EDGE('',*,*,#3512,.T.);
#4709=ORIENTED_EDGE('',*,*,#3513,.T.);
#4710=ORIENTED_EDGE('',*,*,#3512,.F.);
#4711=ORIENTED_EDGE('',*,*,#3514,.T.);
#4712=ORIENTED_EDGE('',*,*,#3513,.F.);
#4713=ORIENTED_EDGE('',*,*,#3514,.F.);
#4714=ORIENTED_EDGE('',*,*,#3515,.T.);
#4715=ORIENTED_EDGE('',*,*,#3516,.T.);
#4716=ORIENTED_EDGE('',*,*,#3515,.F.);
#4717=ORIENTED_EDGE('',*,*,#3516,.F.);
#4718=ORIENTED_EDGE('',*,*,#3517,.T.);
#4719=ORIENTED_EDGE('',*,*,#3517,.F.);
#4720=ORIENTED_EDGE('',*,*,#3518,.T.);
#4721=ORIENTED_EDGE('',*,*,#3519,.T.);
#4722=ORIENTED_EDGE('',*,*,#3518,.F.);
#4723=ORIENTED_EDGE('',*,*,#3519,.F.);
#4724=ORIENTED_EDGE('',*,*,#3520,.T.);
#4725=ORIENTED_EDGE('',*,*,#3521,.F.);
#4726=ORIENTED_EDGE('',*,*,#3522,.F.);
#4727=ORIENTED_EDGE('',*,*,#3523,.F.);
#4728=ORIENTED_EDGE('',*,*,#3524,.F.);
#4729=ORIENTED_EDGE('',*,*,#3525,.F.);
#4730=ORIENTED_EDGE('',*,*,#3526,.F.);
#4731=ORIENTED_EDGE('',*,*,#3527,.F.);
#4732=ORIENTED_EDGE('',*,*,#3528,.F.);
#4733=ORIENTED_EDGE('',*,*,#3520,.F.);
#4734=ORIENTED_EDGE('',*,*,#3529,.T.);
#4735=ORIENTED_EDGE('',*,*,#3530,.T.);
#4736=ORIENTED_EDGE('',*,*,#3529,.F.);
#4737=ORIENTED_EDGE('',*,*,#3530,.F.);
#4738=ORIENTED_EDGE('',*,*,#3531,.T.);
#4739=ORIENTED_EDGE('',*,*,#3531,.F.);
#4740=ORIENTED_EDGE('',*,*,#3532,.T.);
#4741=ORIENTED_EDGE('',*,*,#3497,.F.);
#4742=ORIENTED_EDGE('',*,*,#3532,.F.);
#4743=ORIENTED_EDGE('',*,*,#3533,.T.);
#4744=ORIENTED_EDGE('',*,*,#3534,.T.);
#4745=ORIENTED_EDGE('',*,*,#3535,.T.);
#4746=ORIENTED_EDGE('',*,*,#3534,.F.);
#4747=ORIENTED_EDGE('',*,*,#3535,.F.);
#4748=ORIENTED_EDGE('',*,*,#3536,.T.);
#4749=ORIENTED_EDGE('',*,*,#3502,.F.);
#4750=ORIENTED_EDGE('',*,*,#3536,.F.);
#4751=ORIENTED_EDGE('',*,*,#3500,.F.);
#4752=ORIENTED_EDGE('',*,*,#3501,.F.);
#4753=ORIENTED_EDGE('',*,*,#3537,.T.);
#4754=ORIENTED_EDGE('',*,*,#3533,.F.);
#4755=ORIENTED_EDGE('',*,*,#3537,.F.);
#4756=ORIENTED_EDGE('',*,*,#3504,.F.);
#4757=ORIENTED_EDGE('',*,*,#3538,.T.);
#4758=ORIENTED_EDGE('',*,*,#3521,.T.);
#4759=ORIENTED_EDGE('',*,*,#3538,.F.);
#4760=ORIENTED_EDGE('',*,*,#3505,.F.);
#4761=ORIENTED_EDGE('',*,*,#3539,.T.);
#4762=ORIENTED_EDGE('',*,*,#3522,.T.);
#4763=ORIENTED_EDGE('',*,*,#3539,.F.);
#4764=ORIENTED_EDGE('',*,*,#3506,.F.);
#4765=ORIENTED_EDGE('',*,*,#3540,.T.);
#4766=ORIENTED_EDGE('',*,*,#3523,.T.);
#4767=ORIENTED_EDGE('',*,*,#3540,.F.);
#4768=ORIENTED_EDGE('',*,*,#3507,.F.);
#4769=ORIENTED_EDGE('',*,*,#3541,.T.);
#4770=ORIENTED_EDGE('',*,*,#3524,.T.);
#4771=ORIENTED_EDGE('',*,*,#3541,.F.);
#4772=ORIENTED_EDGE('',*,*,#3508,.F.);
#4773=ORIENTED_EDGE('',*,*,#3542,.T.);
#4774=ORIENTED_EDGE('',*,*,#3525,.T.);
#4775=ORIENTED_EDGE('',*,*,#3542,.F.);
#4776=ORIENTED_EDGE('',*,*,#3509,.F.);
#4777=ORIENTED_EDGE('',*,*,#3543,.T.);
#4778=ORIENTED_EDGE('',*,*,#3526,.T.);
#4779=ORIENTED_EDGE('',*,*,#3543,.F.);
#4780=ORIENTED_EDGE('',*,*,#3510,.F.);
#4781=ORIENTED_EDGE('',*,*,#3544,.T.);
#4782=ORIENTED_EDGE('',*,*,#3527,.T.);
#4783=ORIENTED_EDGE('',*,*,#3544,.F.);
#4784=ORIENTED_EDGE('',*,*,#3511,.F.);
#4785=ORIENTED_EDGE('',*,*,#3545,.T.);
#4786=ORIENTED_EDGE('',*,*,#3528,.T.);
#4787=ORIENTED_EDGE('',*,*,#3545,.F.);
#4788=ORIENTED_EDGE('',*,*,#3546,.F.);
#4789=ORIENTED_EDGE('',*,*,#3547,.T.);
#4790=ORIENTED_EDGE('',*,*,#3548,.T.);
#4791=ORIENTED_EDGE('',*,*,#3549,.T.);
#4792=ORIENTED_EDGE('',*,*,#3550,.T.);
#4793=ORIENTED_EDGE('',*,*,#3551,.T.);
#4794=ORIENTED_EDGE('',*,*,#3552,.F.);
#4795=ORIENTED_EDGE('',*,*,#3553,.F.);
#4796=ORIENTED_EDGE('',*,*,#3554,.F.);
#4797=ORIENTED_EDGE('',*,*,#3555,.T.);
#4798=ORIENTED_EDGE('',*,*,#3547,.F.);
#4799=ORIENTED_EDGE('',*,*,#3556,.T.);
#4800=ORIENTED_EDGE('',*,*,#3557,.T.);
#4801=ORIENTED_EDGE('',*,*,#3558,.T.);
#4802=ORIENTED_EDGE('',*,*,#3559,.T.);
#4803=ORIENTED_EDGE('',*,*,#3560,.F.);
#4804=ORIENTED_EDGE('',*,*,#3561,.F.);
#4805=ORIENTED_EDGE('',*,*,#3561,.T.);
#4806=ORIENTED_EDGE('',*,*,#3562,.T.);
#4807=ORIENTED_EDGE('',*,*,#3563,.F.);
#4808=ORIENTED_EDGE('',*,*,#3562,.F.);
#4809=ORIENTED_EDGE('',*,*,#3564,.F.);
#4810=ORIENTED_EDGE('',*,*,#3565,.T.);
#4811=ORIENTED_EDGE('',*,*,#3566,.T.);
#4812=ORIENTED_EDGE('',*,*,#3567,.T.);
#4813=ORIENTED_EDGE('',*,*,#3563,.T.);
#4814=ORIENTED_EDGE('',*,*,#3564,.T.);
#4815=ORIENTED_EDGE('',*,*,#3568,.F.);
#4816=ORIENTED_EDGE('',*,*,#3569,.F.);
#4817=ORIENTED_EDGE('',*,*,#3549,.F.);
#4818=ORIENTED_EDGE('',*,*,#3570,.F.);
#4819=ORIENTED_EDGE('',*,*,#3571,.F.);
#4820=ORIENTED_EDGE('',*,*,#3572,.F.);
#4821=ORIENTED_EDGE('',*,*,#3573,.T.);
#4822=ORIENTED_EDGE('',*,*,#3565,.F.);
#4823=ORIENTED_EDGE('',*,*,#3571,.T.);
#4824=ORIENTED_EDGE('',*,*,#3574,.T.);
#4825=ORIENTED_EDGE('',*,*,#3575,.F.);
#4826=ORIENTED_EDGE('',*,*,#3559,.F.);
#4827=ORIENTED_EDGE('',*,*,#3576,.T.);
#4828=ORIENTED_EDGE('',*,*,#3572,.T.);
#4829=ORIENTED_EDGE('',*,*,#3577,.F.);
#4830=ORIENTED_EDGE('',*,*,#3556,.F.);
#4831=ORIENTED_EDGE('',*,*,#3577,.T.);
#4832=ORIENTED_EDGE('',*,*,#3578,.T.);
#4833=ORIENTED_EDGE('',*,*,#3553,.T.);
#4834=ORIENTED_EDGE('',*,*,#3579,.F.);
#4835=ORIENTED_EDGE('',*,*,#3557,.F.);
#4836=ORIENTED_EDGE('',*,*,#3579,.T.);
#4837=ORIENTED_EDGE('',*,*,#3580,.T.);
#4838=ORIENTED_EDGE('',*,*,#3581,.F.);
#4839=ORIENTED_EDGE('',*,*,#3558,.F.);
#4840=ORIENTED_EDGE('',*,*,#3581,.T.);
#4841=ORIENTED_EDGE('',*,*,#3582,.T.);
#4842=ORIENTED_EDGE('',*,*,#3576,.F.);
#4843=ORIENTED_EDGE('',*,*,#3582,.F.);
#4844=ORIENTED_EDGE('',*,*,#3583,.T.);
#4845=ORIENTED_EDGE('',*,*,#3566,.F.);
#4846=ORIENTED_EDGE('',*,*,#3573,.F.);
#4847=ORIENTED_EDGE('',*,*,#3580,.F.);
#4848=ORIENTED_EDGE('',*,*,#3552,.T.);
#4849=ORIENTED_EDGE('',*,*,#3584,.F.);
#4850=ORIENTED_EDGE('',*,*,#3568,.T.);
#4851=ORIENTED_EDGE('',*,*,#3567,.F.);
#4852=ORIENTED_EDGE('',*,*,#3583,.F.);
#4853=ORIENTED_EDGE('',*,*,#3585,.F.);
#4854=ORIENTED_EDGE('',*,*,#3574,.F.);
#4855=ORIENTED_EDGE('',*,*,#3570,.T.);
#4856=ORIENTED_EDGE('',*,*,#3548,.F.);
#4857=ORIENTED_EDGE('',*,*,#3586,.T.);
#4858=ORIENTED_EDGE('',*,*,#3587,.F.);
#4859=ORIENTED_EDGE('',*,*,#3588,.F.);
#4860=ORIENTED_EDGE('',*,*,#3586,.F.);
#4861=ORIENTED_EDGE('',*,*,#3555,.F.);
#4862=ORIENTED_EDGE('',*,*,#3589,.F.);
#4863=ORIENTED_EDGE('',*,*,#3590,.F.);
#4864=ORIENTED_EDGE('',*,*,#3591,.T.);
#4865=ORIENTED_EDGE('',*,*,#3550,.F.);
#4866=ORIENTED_EDGE('',*,*,#3569,.T.);
#4867=ORIENTED_EDGE('',*,*,#3584,.T.);
#4868=ORIENTED_EDGE('',*,*,#3551,.F.);
#4869=ORIENTED_EDGE('',*,*,#3591,.F.);
#4870=ORIENTED_EDGE('',*,*,#3554,.T.);
#4871=ORIENTED_EDGE('',*,*,#3578,.F.);
#4872=ORIENTED_EDGE('',*,*,#3575,.T.);
#4873=ORIENTED_EDGE('',*,*,#3585,.T.);
#4874=ORIENTED_EDGE('',*,*,#3560,.T.);
#4875=ORIENTED_EDGE('',*,*,#3592,.T.);
#4876=ORIENTED_EDGE('',*,*,#3587,.T.);
#4877=ORIENTED_EDGE('',*,*,#3593,.T.);
#4878=ORIENTED_EDGE('',*,*,#3594,.F.);
#4879=ORIENTED_EDGE('',*,*,#3593,.F.);
#4880=ORIENTED_EDGE('',*,*,#3588,.T.);
#4881=ORIENTED_EDGE('',*,*,#3592,.F.);
#4882=ORIENTED_EDGE('',*,*,#3589,.T.);
#4883=ORIENTED_EDGE('',*,*,#3590,.T.);
#4884=ORIENTED_EDGE('',*,*,#3546,.T.);
#4885=ORIENTED_EDGE('',*,*,#3594,.T.);
#4886=ORIENTED_EDGE('',*,*,#3595,.F.);
#4887=ORIENTED_EDGE('',*,*,#3596,.T.);
#4888=ORIENTED_EDGE('',*,*,#3597,.T.);
#4889=ORIENTED_EDGE('',*,*,#3596,.F.);
#4890=ORIENTED_EDGE('',*,*,#3597,.F.);
#4891=ORIENTED_EDGE('',*,*,#3598,.F.);
#4892=ORIENTED_EDGE('',*,*,#3599,.F.);
#4893=ORIENTED_EDGE('',*,*,#3599,.T.);
#4894=ORIENTED_EDGE('',*,*,#3600,.T.);
#4895=ORIENTED_EDGE('',*,*,#3601,.T.);
#4896=ORIENTED_EDGE('',*,*,#3600,.F.);
#4897=ORIENTED_EDGE('',*,*,#3602,.F.);
#4898=ORIENTED_EDGE('',*,*,#3601,.F.);
#4899=ORIENTED_EDGE('',*,*,#3602,.T.);
#4900=ORIENTED_EDGE('',*,*,#3603,.T.);
#4901=ORIENTED_EDGE('',*,*,#3604,.T.);
#4902=ORIENTED_EDGE('',*,*,#3603,.F.);
#4903=ORIENTED_EDGE('',*,*,#3605,.F.);
#4904=ORIENTED_EDGE('',*,*,#3604,.F.);
#4905=ORIENTED_EDGE('',*,*,#3605,.T.);
#4906=ORIENTED_EDGE('',*,*,#3606,.T.);
#4907=ORIENTED_EDGE('',*,*,#3607,.T.);
#4908=ORIENTED_EDGE('',*,*,#3608,.T.);
#4909=ORIENTED_EDGE('',*,*,#3609,.T.);
#4910=ORIENTED_EDGE('',*,*,#3610,.F.);
#4911=ORIENTED_EDGE('',*,*,#3611,.F.);
#4912=ORIENTED_EDGE('',*,*,#3612,.T.);
#4913=ORIENTED_EDGE('',*,*,#3613,.T.);
#4914=ORIENTED_EDGE('',*,*,#3614,.F.);
#4915=ORIENTED_EDGE('',*,*,#3615,.T.);
#4916=ORIENTED_EDGE('',*,*,#3606,.F.);
#4917=ORIENTED_EDGE('',*,*,#3610,.T.);
#4918=ORIENTED_EDGE('',*,*,#3616,.F.);
#4919=ORIENTED_EDGE('',*,*,#3612,.F.);
#4920=ORIENTED_EDGE('',*,*,#3617,.F.);
#4921=ORIENTED_EDGE('',*,*,#3609,.F.);
#4922=ORIENTED_EDGE('',*,*,#3618,.F.);
#4923=ORIENTED_EDGE('',*,*,#3613,.F.);
#4924=ORIENTED_EDGE('',*,*,#3616,.T.);
#4925=ORIENTED_EDGE('',*,*,#3608,.F.);
#4926=ORIENTED_EDGE('',*,*,#3619,.T.);
#4927=ORIENTED_EDGE('',*,*,#3614,.T.);
#4928=ORIENTED_EDGE('',*,*,#3618,.T.);
#4929=ORIENTED_EDGE('',*,*,#3617,.T.);
#4930=ORIENTED_EDGE('',*,*,#3611,.T.);
#4931=ORIENTED_EDGE('',*,*,#3619,.F.);
#4932=ORIENTED_EDGE('',*,*,#3607,.F.);
#4933=ORIENTED_EDGE('',*,*,#3615,.F.);
#4934=ORIENTED_EDGE('',*,*,#3620,.F.);
#4935=ORIENTED_EDGE('',*,*,#3621,.T.);
#4936=ORIENTED_EDGE('',*,*,#3622,.T.);
#4937=ORIENTED_EDGE('',*,*,#3621,.F.);
#4938=ORIENTED_EDGE('',*,*,#3623,.F.);
#4939=ORIENTED_EDGE('',*,*,#3622,.F.);
#4940=ORIENTED_EDGE('',*,*,#3624,.F.);
#4941=ORIENTED_EDGE('',*,*,#3625,.F.);
#4942=ORIENTED_EDGE('',*,*,#3626,.T.);
#4943=ORIENTED_EDGE('',*,*,#3627,.F.);
#4944=ORIENTED_EDGE('',*,*,#3628,.T.);
#4945=ORIENTED_EDGE('',*,*,#3629,.F.);
#4946=ORIENTED_EDGE('',*,*,#3630,.T.);
#4947=ORIENTED_EDGE('',*,*,#3624,.T.);
#4948=ORIENTED_EDGE('',*,*,#3630,.F.);
#4949=ORIENTED_EDGE('',*,*,#3631,.F.);
#4950=ORIENTED_EDGE('',*,*,#3628,.F.);
#4951=ORIENTED_EDGE('',*,*,#3632,.F.);
#4952=ORIENTED_EDGE('',*,*,#3626,.F.);
#4953=ORIENTED_EDGE('',*,*,#3633,.F.);
#4954=ORIENTED_EDGE('',*,*,#3634,.F.);
#4955=ORIENTED_EDGE('',*,*,#3635,.F.);
#4956=ORIENTED_EDGE('',*,*,#3636,.F.);
#4957=ORIENTED_EDGE('',*,*,#3637,.T.);
#4958=ORIENTED_EDGE('',*,*,#3634,.T.);
#4959=ORIENTED_EDGE('',*,*,#3633,.T.);
#4960=ORIENTED_EDGE('',*,*,#3637,.F.);
#4961=ORIENTED_EDGE('',*,*,#3627,.T.);
#4962=ORIENTED_EDGE('',*,*,#3638,.T.);
#4963=ORIENTED_EDGE('',*,*,#3639,.T.);
#4964=ORIENTED_EDGE('',*,*,#3638,.F.);
#4965=ORIENTED_EDGE('',*,*,#3632,.T.);
#4966=ORIENTED_EDGE('',*,*,#3625,.T.);
#4967=ORIENTED_EDGE('',*,*,#3629,.T.);
#4968=ORIENTED_EDGE('',*,*,#3640,.T.);
#4969=ORIENTED_EDGE('',*,*,#3641,.T.);
#4970=ORIENTED_EDGE('',*,*,#3640,.F.);
#4971=ORIENTED_EDGE('',*,*,#3631,.T.);
#4972=ORIENTED_EDGE('',*,*,#3642,.F.);
#4973=ORIENTED_EDGE('',*,*,#3643,.T.);
#4974=ORIENTED_EDGE('',*,*,#3635,.T.);
#4975=ORIENTED_EDGE('',*,*,#3643,.F.);
#4976=ORIENTED_EDGE('',*,*,#3636,.T.);
#4977=ORIENTED_EDGE('',*,*,#3642,.T.);
#4978=ORIENTED_EDGE('',*,*,#3639,.F.);
#4979=ORIENTED_EDGE('',*,*,#3641,.F.);
#4980=ORIENTED_EDGE('',*,*,#3644,.T.);
#4981=ORIENTED_EDGE('',*,*,#3645,.F.);
#4982=ORIENTED_EDGE('',*,*,#3646,.T.);
#4983=ORIENTED_EDGE('',*,*,#3647,.T.);
#4984=ORIENTED_EDGE('',*,*,#3648,.F.);
#4985=ORIENTED_EDGE('',*,*,#3644,.F.);
#4986=ORIENTED_EDGE('',*,*,#3649,.T.);
#4987=ORIENTED_EDGE('',*,*,#3650,.T.);
#4988=ORIENTED_EDGE('',*,*,#3648,.T.);
#4989=ORIENTED_EDGE('',*,*,#3651,.T.);
#4990=ORIENTED_EDGE('',*,*,#3652,.T.);
#4991=ORIENTED_EDGE('',*,*,#3653,.T.);
#4992=ORIENTED_EDGE('',*,*,#3654,.T.);
#4993=ORIENTED_EDGE('',*,*,#3645,.T.);
#4994=ORIENTED_EDGE('',*,*,#3655,.F.);
#4995=ORIENTED_EDGE('',*,*,#3656,.F.);
#4996=ORIENTED_EDGE('',*,*,#3657,.F.);
#4997=ORIENTED_EDGE('',*,*,#3658,.F.);
#4998=ORIENTED_EDGE('',*,*,#3659,.T.);
#4999=ORIENTED_EDGE('',*,*,#3656,.T.);
#5000=ORIENTED_EDGE('',*,*,#3659,.F.);
#5001=ORIENTED_EDGE('',*,*,#3660,.F.);
#5002=ORIENTED_EDGE('',*,*,#3661,.T.);
#5003=ORIENTED_EDGE('',*,*,#3662,.T.);
#5004=ORIENTED_EDGE('',*,*,#3661,.F.);
#5005=ORIENTED_EDGE('',*,*,#3657,.T.);
#5006=ORIENTED_EDGE('',*,*,#3658,.T.);
#5007=ORIENTED_EDGE('',*,*,#3663,.T.);
#5008=ORIENTED_EDGE('',*,*,#3664,.T.);
#5009=ORIENTED_EDGE('',*,*,#3665,.F.);
#5010=ORIENTED_EDGE('',*,*,#3662,.F.);
#5011=ORIENTED_EDGE('',*,*,#3666,.F.);
#5012=ORIENTED_EDGE('',*,*,#3667,.F.);
#5013=ORIENTED_EDGE('',*,*,#3668,.F.);
#5014=ORIENTED_EDGE('',*,*,#3665,.T.);
#5015=ORIENTED_EDGE('',*,*,#3669,.T.);
#5016=ORIENTED_EDGE('',*,*,#3670,.T.);
#5017=ORIENTED_EDGE('',*,*,#3671,.T.);
#5018=ORIENTED_EDGE('',*,*,#3669,.F.);
#5019=ORIENTED_EDGE('',*,*,#3670,.F.);
#5020=ORIENTED_EDGE('',*,*,#3671,.F.);
#5021=ORIENTED_EDGE('',*,*,#3672,.T.);
#5022=ORIENTED_EDGE('',*,*,#3673,.T.);
#5023=ORIENTED_EDGE('',*,*,#3672,.F.);
#5024=ORIENTED_EDGE('',*,*,#3673,.F.);
#5025=ORIENTED_EDGE('',*,*,#3674,.T.);
#5026=ORIENTED_EDGE('',*,*,#3675,.T.);
#5027=ORIENTED_EDGE('',*,*,#3676,.F.);
#5028=ORIENTED_EDGE('',*,*,#3677,.T.);
#5029=ORIENTED_EDGE('',*,*,#3677,.F.);
#5030=ORIENTED_EDGE('',*,*,#3678,.T.);
#5031=ORIENTED_EDGE('',*,*,#3666,.T.);
#5032=ORIENTED_EDGE('',*,*,#3678,.F.);
#5033=ORIENTED_EDGE('',*,*,#3674,.F.);
#5034=ORIENTED_EDGE('',*,*,#3679,.T.);
#5035=ORIENTED_EDGE('',*,*,#3667,.T.);
#5036=ORIENTED_EDGE('',*,*,#3679,.F.);
#5037=ORIENTED_EDGE('',*,*,#3675,.F.);
#5038=ORIENTED_EDGE('',*,*,#3680,.T.);
#5039=ORIENTED_EDGE('',*,*,#3668,.T.);
#5040=ORIENTED_EDGE('',*,*,#3680,.F.);
#5041=ORIENTED_EDGE('',*,*,#3676,.T.);
#5042=ORIENTED_EDGE('',*,*,#3681,.T.);
#5043=ORIENTED_EDGE('',*,*,#3682,.F.);
#5044=ORIENTED_EDGE('',*,*,#3683,.F.);
#5045=ORIENTED_EDGE('',*,*,#3681,.F.);
#5046=ORIENTED_EDGE('',*,*,#3682,.T.);
#5047=ORIENTED_EDGE('',*,*,#3683,.T.);
#5048=ORIENTED_EDGE('',*,*,#3684,.T.);
#5049=ORIENTED_EDGE('',*,*,#3685,.T.);
#5050=ORIENTED_EDGE('',*,*,#3686,.T.);
#5051=ORIENTED_EDGE('',*,*,#3687,.F.);
#5052=ORIENTED_EDGE('',*,*,#3688,.T.);
#5053=ORIENTED_EDGE('',*,*,#3684,.F.);
#5054=ORIENTED_EDGE('',*,*,#3689,.T.);
#5055=ORIENTED_EDGE('',*,*,#3663,.F.);
#5056=ORIENTED_EDGE('',*,*,#3664,.F.);
#5057=ORIENTED_EDGE('',*,*,#3690,.T.);
#5058=ORIENTED_EDGE('',*,*,#3689,.F.);
#5059=ORIENTED_EDGE('',*,*,#3690,.F.);
#5060=ORIENTED_EDGE('',*,*,#3691,.F.);
#5061=ORIENTED_EDGE('',*,*,#3692,.F.);
#5062=ORIENTED_EDGE('',*,*,#3685,.F.);
#5063=ORIENTED_EDGE('',*,*,#3693,.F.);
#5064=ORIENTED_EDGE('',*,*,#3691,.T.);
#5065=ORIENTED_EDGE('',*,*,#3694,.F.);
#5066=ORIENTED_EDGE('',*,*,#3652,.F.);
#5067=ORIENTED_EDGE('',*,*,#3695,.T.);
#5068=ORIENTED_EDGE('',*,*,#3650,.F.);
#5069=ORIENTED_EDGE('',*,*,#3686,.F.);
#5070=ORIENTED_EDGE('',*,*,#3692,.T.);
#5071=ORIENTED_EDGE('',*,*,#3695,.F.);
#5072=ORIENTED_EDGE('',*,*,#3651,.F.);
#5073=ORIENTED_EDGE('',*,*,#3647,.F.);
#5074=ORIENTED_EDGE('',*,*,#3696,.T.);
#5075=ORIENTED_EDGE('',*,*,#3687,.T.);
#5076=ORIENTED_EDGE('',*,*,#3649,.F.);
#5077=ORIENTED_EDGE('',*,*,#3654,.F.);
#5078=ORIENTED_EDGE('',*,*,#3697,.T.);
#5079=ORIENTED_EDGE('',*,*,#3696,.F.);
#5080=ORIENTED_EDGE('',*,*,#3646,.F.);
#5081=ORIENTED_EDGE('',*,*,#3697,.F.);
#5082=ORIENTED_EDGE('',*,*,#3653,.F.);
#5083=ORIENTED_EDGE('',*,*,#3694,.T.);
#5084=ORIENTED_EDGE('',*,*,#3693,.T.);
#5085=ORIENTED_EDGE('',*,*,#3688,.F.);
#5086=ORIENTED_EDGE('',*,*,#3660,.T.);
#5087=ORIENTED_EDGE('',*,*,#3698,.F.);
#5088=ORIENTED_EDGE('',*,*,#3699,.T.);
#5089=ORIENTED_EDGE('',*,*,#3655,.T.);
#5090=ORIENTED_EDGE('',*,*,#3699,.F.);
#5091=ORIENTED_EDGE('',*,*,#3698,.T.);
#5092=ORIENTED_EDGE('',*,*,#3700,.F.);
#5093=ORIENTED_EDGE('',*,*,#3701,.T.);
#5094=ORIENTED_EDGE('',*,*,#3702,.T.);
#5095=ORIENTED_EDGE('',*,*,#3701,.F.);
#5096=ORIENTED_EDGE('',*,*,#3702,.F.);
#5097=ORIENTED_EDGE('',*,*,#3703,.F.);
#5098=ORIENTED_EDGE('',*,*,#3704,.F.);
#5099=ORIENTED_EDGE('',*,*,#3705,.T.);
#5100=ORIENTED_EDGE('',*,*,#3706,.T.);
#5101=ORIENTED_EDGE('',*,*,#3705,.F.);
#5102=ORIENTED_EDGE('',*,*,#3706,.F.);
#5103=ORIENTED_EDGE('',*,*,#3707,.F.);
#5104=ORIENTED_EDGE('',*,*,#3708,.F.);
#5105=ORIENTED_EDGE('',*,*,#3709,.T.);
#5106=ORIENTED_EDGE('',*,*,#3710,.T.);
#5107=ORIENTED_EDGE('',*,*,#3709,.F.);
#5108=ORIENTED_EDGE('',*,*,#3710,.F.);
#5109=ORIENTED_EDGE('',*,*,#3711,.F.);
#5110=ORIENTED_EDGE('',*,*,#3712,.F.);
#5111=ORIENTED_EDGE('',*,*,#3713,.T.);
#5112=ORIENTED_EDGE('',*,*,#3714,.T.);
#5113=ORIENTED_EDGE('',*,*,#3713,.F.);
#5114=ORIENTED_EDGE('',*,*,#3714,.F.);
#5115=ORIENTED_EDGE('',*,*,#3715,.F.);
#5116=ORIENTED_EDGE('',*,*,#3716,.F.);
#5117=ORIENTED_EDGE('',*,*,#3717,.T.);
#5118=ORIENTED_EDGE('',*,*,#3718,.T.);
#5119=ORIENTED_EDGE('',*,*,#3717,.F.);
#5120=ORIENTED_EDGE('',*,*,#3719,.F.);
#5121=ORIENTED_EDGE('',*,*,#3718,.F.);
#5122=ORIENTED_EDGE('',*,*,#3720,.T.);
#5123=ORIENTED_EDGE('',*,*,#3721,.T.);
#5124=ORIENTED_EDGE('',*,*,#3722,.T.);
#5125=ORIENTED_EDGE('',*,*,#3723,.T.);
#5126=ORIENTED_EDGE('',*,*,#3724,.T.);
#5127=ORIENTED_EDGE('',*,*,#3721,.F.);
#5128=ORIENTED_EDGE('',*,*,#3725,.T.);
#5129=ORIENTED_EDGE('',*,*,#3726,.T.);
#5130=ORIENTED_EDGE('',*,*,#3725,.F.);
#5131=ORIENTED_EDGE('',*,*,#3726,.F.);
#5132=ORIENTED_EDGE('',*,*,#3727,.T.);
#5133=ORIENTED_EDGE('',*,*,#3727,.F.);
#5134=ORIENTED_EDGE('',*,*,#3728,.T.);
#5135=ORIENTED_EDGE('',*,*,#3729,.T.);
#5136=ORIENTED_EDGE('',*,*,#3728,.F.);
#5137=ORIENTED_EDGE('',*,*,#3730,.T.);
#5138=ORIENTED_EDGE('',*,*,#3729,.F.);
#5139=ORIENTED_EDGE('',*,*,#3730,.F.);
#5140=ORIENTED_EDGE('',*,*,#3731,.T.);
#5141=ORIENTED_EDGE('',*,*,#3732,.T.);
#5142=ORIENTED_EDGE('',*,*,#3733,.T.);
#5143=ORIENTED_EDGE('',*,*,#3731,.F.);
#5144=ORIENTED_EDGE('',*,*,#3733,.F.);
#5145=ORIENTED_EDGE('',*,*,#3734,.T.);
#5146=ORIENTED_EDGE('',*,*,#3735,.F.);
#5147=ORIENTED_EDGE('',*,*,#3734,.F.);
#5148=ORIENTED_EDGE('',*,*,#3732,.F.);
#5149=ORIENTED_EDGE('',*,*,#3736,.T.);
#5150=ORIENTED_EDGE('',*,*,#3737,.F.);
#5151=ORIENTED_EDGE('',*,*,#3738,.F.);
#5152=ORIENTED_EDGE('',*,*,#3739,.F.);
#5153=ORIENTED_EDGE('',*,*,#3735,.T.);
#5154=ORIENTED_EDGE('',*,*,#3722,.F.);
#5155=ORIENTED_EDGE('',*,*,#3740,.T.);
#5156=ORIENTED_EDGE('',*,*,#3737,.T.);
#5157=ORIENTED_EDGE('',*,*,#3740,.F.);
#5158=ORIENTED_EDGE('',*,*,#3723,.F.);
#5159=ORIENTED_EDGE('',*,*,#3741,.T.);
#5160=ORIENTED_EDGE('',*,*,#3738,.T.);
#5161=ORIENTED_EDGE('',*,*,#3741,.F.);
#5162=ORIENTED_EDGE('',*,*,#3724,.F.);
#5163=ORIENTED_EDGE('',*,*,#3742,.T.);
#5164=ORIENTED_EDGE('',*,*,#3739,.T.);
#5165=ORIENTED_EDGE('',*,*,#3742,.F.);
#5166=ORIENTED_EDGE('',*,*,#3736,.F.);
#5167=ORIENTED_EDGE('',*,*,#3743,.T.);
#5168=ORIENTED_EDGE('',*,*,#3744,.T.);
#5169=ORIENTED_EDGE('',*,*,#3745,.T.);
#5170=ORIENTED_EDGE('',*,*,#3743,.F.);
#5171=ORIENTED_EDGE('',*,*,#3745,.F.);
#5172=ORIENTED_EDGE('',*,*,#3746,.T.);
#5173=ORIENTED_EDGE('',*,*,#3720,.F.);
#5174=ORIENTED_EDGE('',*,*,#3746,.F.);
#5175=ORIENTED_EDGE('',*,*,#3744,.F.);
#5176=ORIENTED_EDGE('',*,*,#3747,.F.);
#5177=ORIENTED_EDGE('',*,*,#3748,.F.);
#5178=ORIENTED_EDGE('',*,*,#3747,.T.);
#5179=ORIENTED_EDGE('',*,*,#3749,.T.);
#5180=ORIENTED_EDGE('',*,*,#3750,.F.);
#5181=ORIENTED_EDGE('',*,*,#3751,.F.);
#5182=ORIENTED_EDGE('',*,*,#3748,.T.);
#5183=ORIENTED_EDGE('',*,*,#3751,.T.);
#5184=ORIENTED_EDGE('',*,*,#3752,.F.);
#5185=ORIENTED_EDGE('',*,*,#3749,.F.);
#5186=ORIENTED_EDGE('',*,*,#3752,.T.);
#5187=ORIENTED_EDGE('',*,*,#3753,.T.);
#5188=ORIENTED_EDGE('',*,*,#3754,.F.);
#5189=ORIENTED_EDGE('',*,*,#3755,.F.);
#5190=ORIENTED_EDGE('',*,*,#3750,.T.);
#5191=ORIENTED_EDGE('',*,*,#3755,.T.);
#5192=ORIENTED_EDGE('',*,*,#3756,.F.);
#5193=ORIENTED_EDGE('',*,*,#3753,.F.);
#5194=ORIENTED_EDGE('',*,*,#3756,.T.);
#5195=ORIENTED_EDGE('',*,*,#3757,.T.);
#5196=ORIENTED_EDGE('',*,*,#3758,.F.);
#5197=ORIENTED_EDGE('',*,*,#3759,.F.);
#5198=ORIENTED_EDGE('',*,*,#3754,.T.);
#5199=ORIENTED_EDGE('',*,*,#3759,.T.);
#5200=ORIENTED_EDGE('',*,*,#3760,.F.);
#5201=ORIENTED_EDGE('',*,*,#3757,.F.);
#5202=ORIENTED_EDGE('',*,*,#3758,.T.);
#5203=ORIENTED_EDGE('',*,*,#3760,.T.);
#5204=ORIENTED_EDGE('',*,*,#3761,.F.);
#5205=ORIENTED_EDGE('',*,*,#3762,.F.);
#5206=ORIENTED_EDGE('',*,*,#3763,.F.);
#5207=ORIENTED_EDGE('',*,*,#3764,.F.);
#5208=ORIENTED_EDGE('',*,*,#3765,.F.);
#5209=ORIENTED_EDGE('',*,*,#3766,.F.);
#5210=ORIENTED_EDGE('',*,*,#3767,.F.);
#5211=ORIENTED_EDGE('',*,*,#3767,.T.);
#5212=ORIENTED_EDGE('',*,*,#3768,.T.);
#5213=ORIENTED_EDGE('',*,*,#3769,.F.);
#5214=ORIENTED_EDGE('',*,*,#3768,.F.);
#5215=ORIENTED_EDGE('',*,*,#3770,.T.);
#5216=ORIENTED_EDGE('',*,*,#3771,.T.);
#5217=ORIENTED_EDGE('',*,*,#3772,.T.);
#5218=ORIENTED_EDGE('',*,*,#3773,.T.);
#5219=ORIENTED_EDGE('',*,*,#3774,.T.);
#5220=ORIENTED_EDGE('',*,*,#3775,.T.);
#5221=ORIENTED_EDGE('',*,*,#3769,.T.);
#5222=ORIENTED_EDGE('',*,*,#3761,.T.);
#5223=ORIENTED_EDGE('',*,*,#3776,.T.);
#5224=ORIENTED_EDGE('',*,*,#3770,.F.);
#5225=ORIENTED_EDGE('',*,*,#3777,.F.);
#5226=ORIENTED_EDGE('',*,*,#3762,.T.);
#5227=ORIENTED_EDGE('',*,*,#3777,.T.);
#5228=ORIENTED_EDGE('',*,*,#3775,.F.);
#5229=ORIENTED_EDGE('',*,*,#3778,.F.);
#5230=ORIENTED_EDGE('',*,*,#3763,.T.);
#5231=ORIENTED_EDGE('',*,*,#3778,.T.);
#5232=ORIENTED_EDGE('',*,*,#3774,.F.);
#5233=ORIENTED_EDGE('',*,*,#3779,.F.);
#5234=ORIENTED_EDGE('',*,*,#3764,.T.);
#5235=ORIENTED_EDGE('',*,*,#3779,.T.);
#5236=ORIENTED_EDGE('',*,*,#3773,.F.);
#5237=ORIENTED_EDGE('',*,*,#3780,.F.);
#5238=ORIENTED_EDGE('',*,*,#3765,.T.);
#5239=ORIENTED_EDGE('',*,*,#3780,.T.);
#5240=ORIENTED_EDGE('',*,*,#3772,.F.);
#5241=ORIENTED_EDGE('',*,*,#3781,.F.);
#5242=ORIENTED_EDGE('',*,*,#3766,.T.);
#5243=ORIENTED_EDGE('',*,*,#3781,.T.);
#5244=ORIENTED_EDGE('',*,*,#3771,.F.);
#5245=ORIENTED_EDGE('',*,*,#3776,.F.);
#5246=ORIENTED_EDGE('',*,*,#3782,.F.);
#5247=ORIENTED_EDGE('',*,*,#3783,.T.);
#5248=ORIENTED_EDGE('',*,*,#3784,.T.);
#5249=ORIENTED_EDGE('',*,*,#3783,.F.);
#5250=ORIENTED_EDGE('',*,*,#3784,.F.);
#5251=ORIENTED_EDGE('',*,*,#3785,.F.);
#5252=ORIENTED_EDGE('',*,*,#3786,.T.);
#5253=ORIENTED_EDGE('',*,*,#3787,.T.);
#5254=ORIENTED_EDGE('',*,*,#3788,.T.);
#5255=ORIENTED_EDGE('',*,*,#3789,.T.);
#5256=ORIENTED_EDGE('',*,*,#3790,.T.);
#5257=ORIENTED_EDGE('',*,*,#3791,.T.);
#5258=ORIENTED_EDGE('',*,*,#3792,.T.);
#5259=ORIENTED_EDGE('',*,*,#3793,.T.);
#5260=ORIENTED_EDGE('',*,*,#3794,.F.);
#5261=ORIENTED_EDGE('',*,*,#3795,.F.);
#5262=ORIENTED_EDGE('',*,*,#3786,.F.);
#5263=ORIENTED_EDGE('',*,*,#3796,.T.);
#5264=ORIENTED_EDGE('',*,*,#3797,.T.);
#5265=ORIENTED_EDGE('',*,*,#3794,.T.);
#5266=ORIENTED_EDGE('',*,*,#3798,.F.);
#5267=ORIENTED_EDGE('',*,*,#3799,.F.);
#5268=ORIENTED_EDGE('',*,*,#3800,.F.);
#5269=ORIENTED_EDGE('',*,*,#3801,.T.);
#5270=ORIENTED_EDGE('',*,*,#3802,.F.);
#5271=ORIENTED_EDGE('',*,*,#3803,.T.);
#5272=ORIENTED_EDGE('',*,*,#3804,.F.);
#5273=ORIENTED_EDGE('',*,*,#3805,.F.);
#5274=ORIENTED_EDGE('',*,*,#3806,.F.);
#5275=ORIENTED_EDGE('',*,*,#3807,.T.);
#5276=ORIENTED_EDGE('',*,*,#3808,.F.);
#5277=ORIENTED_EDGE('',*,*,#3797,.F.);
#5278=ORIENTED_EDGE('',*,*,#3809,.T.);
#5279=ORIENTED_EDGE('',*,*,#3810,.F.);
#5280=ORIENTED_EDGE('',*,*,#3809,.F.);
#5281=ORIENTED_EDGE('',*,*,#3811,.T.);
#5282=ORIENTED_EDGE('',*,*,#3810,.T.);
#5283=ORIENTED_EDGE('',*,*,#3811,.F.);
#5284=ORIENTED_EDGE('',*,*,#3812,.T.);
#5285=ORIENTED_EDGE('',*,*,#3813,.T.);
#5286=ORIENTED_EDGE('',*,*,#3814,.T.);
#5287=ORIENTED_EDGE('',*,*,#3812,.F.);
#5288=ORIENTED_EDGE('',*,*,#3799,.T.);
#5289=ORIENTED_EDGE('',*,*,#3815,.T.);
#5290=ORIENTED_EDGE('',*,*,#3814,.F.);
#5291=ORIENTED_EDGE('',*,*,#3816,.T.);
#5292=ORIENTED_EDGE('',*,*,#3817,.T.);
#5293=ORIENTED_EDGE('',*,*,#3800,.T.);
#5294=ORIENTED_EDGE('',*,*,#3816,.F.);
#5295=ORIENTED_EDGE('',*,*,#3818,.F.);
#5296=ORIENTED_EDGE('',*,*,#3804,.T.);
#5297=ORIENTED_EDGE('',*,*,#3819,.F.);
#5298=ORIENTED_EDGE('',*,*,#3789,.F.);
#5299=ORIENTED_EDGE('',*,*,#3820,.T.);
#5300=ORIENTED_EDGE('',*,*,#3820,.F.);
#5301=ORIENTED_EDGE('',*,*,#3821,.T.);
#5302=ORIENTED_EDGE('',*,*,#3822,.T.);
#5303=ORIENTED_EDGE('',*,*,#3821,.F.);
#5304=ORIENTED_EDGE('',*,*,#3796,.F.);
#5305=ORIENTED_EDGE('',*,*,#3793,.F.);
#5306=ORIENTED_EDGE('',*,*,#3823,.T.);
#5307=ORIENTED_EDGE('',*,*,#3806,.T.);
#5308=ORIENTED_EDGE('',*,*,#3824,.F.);
#5309=ORIENTED_EDGE('',*,*,#3815,.F.);
#5310=ORIENTED_EDGE('',*,*,#3798,.T.);
#5311=ORIENTED_EDGE('',*,*,#3822,.F.);
#5312=ORIENTED_EDGE('',*,*,#3813,.F.);
#5313=ORIENTED_EDGE('',*,*,#3824,.T.);
#5314=ORIENTED_EDGE('',*,*,#3805,.T.);
#5315=ORIENTED_EDGE('',*,*,#3818,.T.);
#5316=ORIENTED_EDGE('',*,*,#3807,.F.);
#5317=ORIENTED_EDGE('',*,*,#3823,.F.);
#5318=ORIENTED_EDGE('',*,*,#3792,.F.);
#5319=ORIENTED_EDGE('',*,*,#3825,.T.);
#5320=ORIENTED_EDGE('',*,*,#3826,.T.);
#5321=ORIENTED_EDGE('',*,*,#3808,.T.);
#5322=ORIENTED_EDGE('',*,*,#3825,.F.);
#5323=ORIENTED_EDGE('',*,*,#3791,.F.);
#5324=ORIENTED_EDGE('',*,*,#3803,.F.);
#5325=ORIENTED_EDGE('',*,*,#3826,.F.);
#5326=ORIENTED_EDGE('',*,*,#3790,.F.);
#5327=ORIENTED_EDGE('',*,*,#3819,.T.);
#5328=ORIENTED_EDGE('',*,*,#3801,.F.);
#5329=ORIENTED_EDGE('',*,*,#3817,.F.);
#5330=ORIENTED_EDGE('',*,*,#3788,.F.);
#5331=ORIENTED_EDGE('',*,*,#3827,.T.);
#5332=ORIENTED_EDGE('',*,*,#3795,.T.);
#5333=ORIENTED_EDGE('',*,*,#3802,.T.);
#5334=ORIENTED_EDGE('',*,*,#3827,.F.);
#5335=ORIENTED_EDGE('',*,*,#3787,.F.);
#5336=ORIENTED_EDGE('',*,*,#3828,.F.);
#5337=ORIENTED_EDGE('',*,*,#3829,.T.);
#5338=ORIENTED_EDGE('',*,*,#3830,.T.);
#5339=ORIENTED_EDGE('',*,*,#3829,.F.);
#5340=ORIENTED_EDGE('',*,*,#3830,.F.);
#5341=ORIENTED_EDGE('',*,*,#3831,.F.);
#5342=ORIENTED_EDGE('',*,*,#3832,.F.);
#5343=ORIENTED_EDGE('',*,*,#3833,.F.);
#5344=ORIENTED_EDGE('',*,*,#3834,.F.);
#5345=ORIENTED_EDGE('',*,*,#3835,.T.);
#5346=ORIENTED_EDGE('',*,*,#3832,.T.);
#5347=ORIENTED_EDGE('',*,*,#3835,.F.);
#5348=ORIENTED_EDGE('',*,*,#3834,.T.);
#5349=ORIENTED_EDGE('',*,*,#3836,.F.);
#5350=ORIENTED_EDGE('',*,*,#3837,.T.);
#5351=ORIENTED_EDGE('',*,*,#3833,.T.);
#5352=ORIENTED_EDGE('',*,*,#3837,.F.);
#5353=ORIENTED_EDGE('',*,*,#3836,.T.);
#5354=ORIENTED_EDGE('',*,*,#3838,.F.);
#5355=ORIENTED_EDGE('',*,*,#3839,.T.);
#5356=ORIENTED_EDGE('',*,*,#3840,.T.);
#5357=ORIENTED_EDGE('',*,*,#3839,.F.);
#5358=ORIENTED_EDGE('',*,*,#3841,.F.);
#5359=ORIENTED_EDGE('',*,*,#3840,.F.);
#5360=ORIENTED_EDGE('',*,*,#3842,.F.);
#5361=ORIENTED_EDGE('',*,*,#3843,.T.);
#5362=ORIENTED_EDGE('',*,*,#3844,.T.);
#5363=ORIENTED_EDGE('',*,*,#3843,.F.);
#5364=ORIENTED_EDGE('',*,*,#3845,.F.);
#5365=ORIENTED_EDGE('',*,*,#3844,.F.);
#5366=ORIENTED_EDGE('',*,*,#3846,.T.);
#5367=ORIENTED_EDGE('',*,*,#3847,.T.);
#5368=ORIENTED_EDGE('',*,*,#3847,.F.);
#5369=ORIENTED_EDGE('',*,*,#3848,.T.);
#5370=ORIENTED_EDGE('',*,*,#3849,.T.);
#5371=ORIENTED_EDGE('',*,*,#3848,.F.);
#5372=ORIENTED_EDGE('',*,*,#3850,.T.);
#5373=ORIENTED_EDGE('',*,*,#3849,.F.);
#5374=ORIENTED_EDGE('',*,*,#3850,.F.);
#5375=ORIENTED_EDGE('',*,*,#3851,.T.);
#5376=ORIENTED_EDGE('',*,*,#3852,.T.);
#5377=ORIENTED_EDGE('',*,*,#3851,.F.);
#5378=ORIENTED_EDGE('',*,*,#3852,.F.);
#5379=ORIENTED_EDGE('',*,*,#3853,.T.);
#5380=ORIENTED_EDGE('',*,*,#3853,.F.);
#5381=ORIENTED_EDGE('',*,*,#3854,.T.);
#5382=ORIENTED_EDGE('',*,*,#3855,.T.);
#5383=ORIENTED_EDGE('',*,*,#3854,.F.);
#5384=ORIENTED_EDGE('',*,*,#3856,.T.);
#5385=ORIENTED_EDGE('',*,*,#3855,.F.);
#5386=ORIENTED_EDGE('',*,*,#3856,.F.);
#5387=ORIENTED_EDGE('',*,*,#3857,.T.);
#5388=ORIENTED_EDGE('',*,*,#3846,.F.);
#5389=ORIENTED_EDGE('',*,*,#3857,.F.);
#5390=ORIENTED_EDGE('',*,*,#3858,.F.);
#5391=ORIENTED_EDGE('',*,*,#3859,.T.);
#5392=ORIENTED_EDGE('',*,*,#3860,.T.);
#5393=ORIENTED_EDGE('',*,*,#3859,.F.);
#5394=ORIENTED_EDGE('',*,*,#3860,.F.);
#5395=ORIENTED_EDGE('',*,*,#3861,.F.);
#5396=ORIENTED_EDGE('',*,*,#3862,.F.);
#5397=ORIENTED_EDGE('',*,*,#3863,.F.);
#5398=ORIENTED_EDGE('',*,*,#3864,.F.);
#5399=ORIENTED_EDGE('',*,*,#3865,.F.);
#5400=ORIENTED_EDGE('',*,*,#3866,.F.);
#5401=ORIENTED_EDGE('',*,*,#3867,.F.);
#5402=ORIENTED_EDGE('',*,*,#3868,.F.);
#5403=ORIENTED_EDGE('',*,*,#3869,.F.);
#5404=ORIENTED_EDGE('',*,*,#3870,.F.);
#5405=ORIENTED_EDGE('',*,*,#3871,.F.);
#5406=ORIENTED_EDGE('',*,*,#3871,.T.);
#5407=ORIENTED_EDGE('',*,*,#3872,.T.);
#5408=ORIENTED_EDGE('',*,*,#3873,.T.);
#5409=ORIENTED_EDGE('',*,*,#3872,.F.);
#5410=ORIENTED_EDGE('',*,*,#3874,.T.);
#5411=ORIENTED_EDGE('',*,*,#3875,.T.);
#5412=ORIENTED_EDGE('',*,*,#3876,.T.);
#5413=ORIENTED_EDGE('',*,*,#3877,.T.);
#5414=ORIENTED_EDGE('',*,*,#3878,.T.);
#5415=ORIENTED_EDGE('',*,*,#3879,.T.);
#5416=ORIENTED_EDGE('',*,*,#3880,.T.);
#5417=ORIENTED_EDGE('',*,*,#3881,.T.);
#5418=ORIENTED_EDGE('',*,*,#3873,.F.);
#5419=ORIENTED_EDGE('',*,*,#3882,.F.);
#5420=ORIENTED_EDGE('',*,*,#3883,.T.);
#5421=ORIENTED_EDGE('',*,*,#3884,.T.);
#5422=ORIENTED_EDGE('',*,*,#3874,.F.);
#5423=ORIENTED_EDGE('',*,*,#3885,.F.);
#5424=ORIENTED_EDGE('',*,*,#3886,.T.);
#5425=ORIENTED_EDGE('',*,*,#3887,.T.);
#5426=ORIENTED_EDGE('',*,*,#3888,.T.);
#5427=ORIENTED_EDGE('',*,*,#3889,.T.);
#5428=ORIENTED_EDGE('',*,*,#3890,.T.);
#5429=ORIENTED_EDGE('',*,*,#3891,.T.);
#5430=ORIENTED_EDGE('',*,*,#3892,.T.);
#5431=ORIENTED_EDGE('',*,*,#3893,.T.);
#5432=ORIENTED_EDGE('',*,*,#3883,.F.);
#5433=ORIENTED_EDGE('',*,*,#3894,.F.);
#5434=ORIENTED_EDGE('',*,*,#3895,.F.);
#5435=ORIENTED_EDGE('',*,*,#3896,.F.);
#5436=ORIENTED_EDGE('',*,*,#3897,.F.);
#5437=ORIENTED_EDGE('',*,*,#3898,.F.);
#5438=ORIENTED_EDGE('',*,*,#3899,.F.);
#5439=ORIENTED_EDGE('',*,*,#3900,.F.);
#5440=ORIENTED_EDGE('',*,*,#3862,.T.);
#5441=ORIENTED_EDGE('',*,*,#3901,.T.);
#5442=ORIENTED_EDGE('',*,*,#3886,.F.);
#5443=ORIENTED_EDGE('',*,*,#3902,.F.);
#5444=ORIENTED_EDGE('',*,*,#3863,.T.);
#5445=ORIENTED_EDGE('',*,*,#3902,.T.);
#5446=ORIENTED_EDGE('',*,*,#3893,.F.);
#5447=ORIENTED_EDGE('',*,*,#3903,.F.);
#5448=ORIENTED_EDGE('',*,*,#3864,.T.);
#5449=ORIENTED_EDGE('',*,*,#3903,.T.);
#5450=ORIENTED_EDGE('',*,*,#3892,.F.);
#5451=ORIENTED_EDGE('',*,*,#3904,.F.);
#5452=ORIENTED_EDGE('',*,*,#3865,.T.);
#5453=ORIENTED_EDGE('',*,*,#3904,.T.);
#5454=ORIENTED_EDGE('',*,*,#3891,.F.);
#5455=ORIENTED_EDGE('',*,*,#3905,.F.);
#5456=ORIENTED_EDGE('',*,*,#3866,.T.);
#5457=ORIENTED_EDGE('',*,*,#3905,.T.);
#5458=ORIENTED_EDGE('',*,*,#3890,.F.);
#5459=ORIENTED_EDGE('',*,*,#3906,.F.);
#5460=ORIENTED_EDGE('',*,*,#3867,.T.);
#5461=ORIENTED_EDGE('',*,*,#3906,.T.);
#5462=ORIENTED_EDGE('',*,*,#3889,.F.);
#5463=ORIENTED_EDGE('',*,*,#3907,.F.);
#5464=ORIENTED_EDGE('',*,*,#3868,.T.);
#5465=ORIENTED_EDGE('',*,*,#3907,.T.);
#5466=ORIENTED_EDGE('',*,*,#3888,.F.);
#5467=ORIENTED_EDGE('',*,*,#3908,.F.);
#5468=ORIENTED_EDGE('',*,*,#3869,.T.);
#5469=ORIENTED_EDGE('',*,*,#3908,.T.);
#5470=ORIENTED_EDGE('',*,*,#3887,.F.);
#5471=ORIENTED_EDGE('',*,*,#3901,.F.);
#5472=ORIENTED_EDGE('',*,*,#3900,.T.);
#5473=ORIENTED_EDGE('',*,*,#3909,.T.);
#5474=ORIENTED_EDGE('',*,*,#3875,.F.);
#5475=ORIENTED_EDGE('',*,*,#3884,.F.);
#5476=ORIENTED_EDGE('',*,*,#3899,.T.);
#5477=ORIENTED_EDGE('',*,*,#3910,.T.);
#5478=ORIENTED_EDGE('',*,*,#3876,.F.);
#5479=ORIENTED_EDGE('',*,*,#3909,.F.);
#5480=ORIENTED_EDGE('',*,*,#3898,.T.);
#5481=ORIENTED_EDGE('',*,*,#3911,.T.);
#5482=ORIENTED_EDGE('',*,*,#3877,.F.);
#5483=ORIENTED_EDGE('',*,*,#3910,.F.);
#5484=ORIENTED_EDGE('',*,*,#3897,.T.);
#5485=ORIENTED_EDGE('',*,*,#3912,.T.);
#5486=ORIENTED_EDGE('',*,*,#3878,.F.);
#5487=ORIENTED_EDGE('',*,*,#3911,.F.);
#5488=ORIENTED_EDGE('',*,*,#3896,.T.);
#5489=ORIENTED_EDGE('',*,*,#3913,.T.);
#5490=ORIENTED_EDGE('',*,*,#3879,.F.);
#5491=ORIENTED_EDGE('',*,*,#3912,.F.);
#5492=ORIENTED_EDGE('',*,*,#3895,.T.);
#5493=ORIENTED_EDGE('',*,*,#3914,.T.);
#5494=ORIENTED_EDGE('',*,*,#3880,.F.);
#5495=ORIENTED_EDGE('',*,*,#3913,.F.);
#5496=ORIENTED_EDGE('',*,*,#3894,.T.);
#5497=ORIENTED_EDGE('',*,*,#3885,.T.);
#5498=ORIENTED_EDGE('',*,*,#3881,.F.);
#5499=ORIENTED_EDGE('',*,*,#3914,.F.);
#5500=ORIENTED_EDGE('',*,*,#3870,.T.);
#5501=ORIENTED_EDGE('',*,*,#3915,.T.);
#5502=ORIENTED_EDGE('',*,*,#3882,.T.);
#5503=ORIENTED_EDGE('',*,*,#3915,.F.);
#5504=PLANE('',#6211);
#5505=PLANE('',#6212);
#5506=PLANE('',#6213);
#5507=PLANE('',#6214);
#5508=PLANE('',#6217);
#5509=PLANE('',#6218);
#5510=PLANE('',#6219);
#5511=PLANE('',#6224);
#5512=PLANE('',#6225);
#5513=PLANE('',#6226);
#5514=PLANE('',#6237);
#5515=PLANE('',#6238);
#5516=PLANE('',#6243);
#5517=PLANE('',#6256);
#5518=PLANE('',#6273);
#5519=PLANE('',#6276);
#5520=PLANE('',#6279);
#5521=PLANE('',#6282);
#5522=PLANE('',#6283);
#5523=PLANE('',#6285);
#5524=PLANE('',#6287);
#5525=PLANE('',#6289);
#5526=PLANE('',#6294);
#5527=PLANE('',#6299);
#5528=PLANE('',#6302);
#5529=PLANE('',#6310);
#5530=PLANE('',#6314);
#5531=PLANE('',#6322);
#5532=PLANE('',#6326);
#5533=PLANE('',#6338);
#5534=PLANE('',#6341);
#5535=PLANE('',#6363);
#5536=PLANE('',#6377);
#5537=PLANE('',#6388);
#5538=PLANE('',#6411);
#5539=PLANE('',#6416);
#5540=PLANE('',#6419);
#5541=PLANE('',#6423);
#5542=PLANE('',#6429);
#5543=PLANE('',#6431);
#5544=PLANE('',#6439);
#5545=PLANE('',#6447);
#5546=PLANE('',#6448);
#5547=PLANE('',#6449);
#5548=PLANE('',#6450);
#5549=PLANE('',#6464);
#5550=PLANE('',#6469);
#5551=PLANE('',#6477);
#5552=PLANE('',#6484);
#5553=PLANE('',#6496);
#5554=PLANE('',#6510);
#5555=PLANE('',#6511);
#5556=PLANE('',#6512);
#5557=PLANE('',#6516);
#5558=PLANE('',#6521);
#5559=PLANE('',#6524);
#5560=PLANE('',#6526);
#5561=PLANE('',#6527);
#5562=PLANE('',#6528);
#5563=PLANE('',#6529);
#5564=PLANE('',#6530);
#5565=PLANE('',#6531);
#5566=PLANE('',#6532);
#5567=PLANE('',#6538);
#5568=PLANE('',#6542);
#5569=PLANE('',#6546);
#5570=PLANE('',#6551);
#5571=PLANE('',#6559);
#5572=PLANE('',#6564);
#5573=PLANE('',#6576);
#5574=PLANE('',#6580);
#5575=PLANE('',#6584);
#5576=PLANE('',#6596);
#5577=PLANE('',#6615);
#5578=PLANE('',#6622);
#5579=PLANE('',#6626);
#5580=PLANE('',#6639);
#5581=PLANE('',#6646);
#5582=PLANE('',#6650);
#5583=PLANE('',#6653);
#5584=PLANE('',#6657);
#5585=PLANE('',#6661);
#5586=PLANE('',#6669);
#5587=PLANE('',#6670);
#5588=PLANE('',#6671);
#5589=PLANE('',#6672);
#5590=PLANE('',#6673);
#5591=PLANE('',#6677);
#5592=PLANE('',#6680);
#5593=PLANE('',#6688);
#5594=PLANE('',#6693);
#5595=PLANE('',#6694);
#5596=PLANE('',#6695);
#5597=PLANE('',#6696);
#5598=PLANE('',#6704);
#5599=PLANE('',#6709);
#5600=PLANE('',#6717);
#5601=PLANE('',#6728);
#5602=PLANE('',#6746);
#5603=PLANE('',#6747);
#5604=PLANE('',#6751);
#5605=PLANE('',#6752);
#5606=PLANE('',#6755);
#5607=PLANE('',#6759);
#5608=PLANE('',#6764);
#5609=PLANE('',#6769);
#5610=PLANE('',#6774);
#5611=PLANE('',#6779);
#5612=PLANE('',#6782);
#5613=PLANE('',#6790);
#5614=PLANE('',#6794);
#5615=PLANE('',#6802);
#5616=PLANE('',#6816);
#5617=PLANE('',#6817);
#5618=PLANE('',#6819);
#5619=PLANE('',#6823);
#5620=PLANE('',#6824);
#5621=PLANE('',#6825);
#5622=PLANE('',#6826);
#5623=PLANE('',#6827);
#5624=PLANE('',#6828);
#5625=PLANE('',#6829);
#5626=PLANE('',#6833);
#5627=PLANE('',#6837);
#5628=PLANE('',#6846);
#5629=PLANE('',#6848);
#5630=PLANE('',#6852);
#5631=PLANE('',#6859);
#5632=PLANE('',#6865);
#5633=PLANE('',#6869);
#5634=PLANE('',#6879);
#5635=PLANE('',#6882);
#5636=PLANE('',#6887);
#5637=PLANE('',#6890);
#5638=PLANE('',#6894);
#5639=PLANE('',#6899);
#5640=PLANE('',#6902);
#5641=PLANE('',#6907);
#5642=PLANE('',#6911);
#5643=PLANE('',#6915);
#5644=PLANE('',#6921);
#5645=PLANE('',#6932);
#5646=PLANE('',#6941);
#5647=PLANE('',#6949);
#5648=PLANE('',#6958);
#5649=PLANE('',#6960);
#5650=PLANE('',#6962);
#5651=PLANE('',#6964);
#5652=PLANE('',#6965);
#5653=PLANE('',#6967);
#5654=PLANE('',#6969);
#5655=PLANE('',#6971);
#5656=ADVANCED_FACE('',(#1008),#5504,.F.);
#5657=ADVANCED_FACE('',(#1009),#5505,.T.);
#5658=ADVANCED_FACE('',(#1010),#5506,.T.);
#5659=ADVANCED_FACE('',(#1011,#504,#505),#5507,.F.);
#5660=ADVANCED_FACE('',(#1012),#5508,.T.);
#5661=ADVANCED_FACE('',(#1013),#5509,.T.);
#5662=ADVANCED_FACE('',(#1014,#506,#507,#508,#509),#5510,.T.);
#5663=ADVANCED_FACE('',(#1015),#5511,.T.);
#5664=ADVANCED_FACE('',(#1016),#5512,.T.);
#5665=ADVANCED_FACE('',(#1017,#510,#511,#512,#513),#5513,.T.);
#5666=ADVANCED_FACE('',(#1018),#346,.F.);
#5667=ADVANCED_FACE('',(#1019),#347,.F.);
#5668=ADVANCED_FACE('',(#1020),#348,.F.);
#5669=ADVANCED_FACE('',(#1021),#349,.F.);
#5670=ADVANCED_FACE('',(#1022),#350,.F.);
#5671=ADVANCED_FACE('',(#1023),#5514,.T.);
#5672=ADVANCED_FACE('',(#1024),#5515,.T.);
#5673=ADVANCED_FACE('',(#1025),#351,.F.);
#5674=ADVANCED_FACE('',(#1026,#514,#515,#516,#517,#518,#519),#5516,.F.);
#5675=ADVANCED_FACE('',(#1027),#352,.F.);
#5676=ADVANCED_FACE('',(#1028,#520,#521,#522,#523,#524,#525),#5517,.T.);
#5677=ADVANCED_FACE('',(#1029),#353,.F.);
#5678=ADVANCED_FACE('',(#1030),#354,.F.);
#5679=ADVANCED_FACE('',(#1031),#355,.F.);
#5680=ADVANCED_FACE('',(#1032),#356,.F.);
#5681=ADVANCED_FACE('',(#1033),#357,.F.);
#5682=ADVANCED_FACE('',(#1034),#257,.T.);
#5683=ADVANCED_FACE('',(#1035),#5518,.T.);
#5684=ADVANCED_FACE('',(#1036),#258,.T.);
#5685=ADVANCED_FACE('',(#1037),#5519,.T.);
#5686=ADVANCED_FACE('',(#1038),#259,.T.);
#5687=ADVANCED_FACE('',(#1039),#5520,.T.);
#5688=ADVANCED_FACE('',(#1040),#260,.T.);
#5689=ADVANCED_FACE('',(#1041),#5521,.T.);
#5690=ADVANCED_FACE('',(#1042),#5522,.T.);
#5691=ADVANCED_FACE('',(#1043),#358,.T.);
#5692=ADVANCED_FACE('',(#1044),#5523,.T.);
#5693=ADVANCED_FACE('',(#1045),#359,.T.);
#5694=ADVANCED_FACE('',(#1046),#5524,.T.);
#5695=ADVANCED_FACE('',(#1047),#360,.T.);
#5696=ADVANCED_FACE('',(#1048),#5525,.T.);
#5697=ADVANCED_FACE('',(#1049),#361,.T.);
#5698=ADVANCED_FACE('',(#1050),#362,.T.);
#5699=ADVANCED_FACE('',(#1051,#526),#5526,.F.);
#5700=ADVANCED_FACE('',(#1052),#363,.T.);
#5701=ADVANCED_FACE('',(#1053,#527),#5527,.F.);
#5702=ADVANCED_FACE('',(#1054,#528),#5528,.F.);
#5703=ADVANCED_FACE('',(#1055),#364,.T.);
#5704=ADVANCED_FACE('',(#1056),#126,.T.);
#5705=ADVANCED_FACE('',(#1057,#529),#5529,.F.);
#5706=ADVANCED_FACE('',(#1058,#530),#365,.F.);
#5707=ADVANCED_FACE('',(#1059,#531),#5530,.T.);
#5708=ADVANCED_FACE('',(#1060),#127,.T.);
#5709=ADVANCED_FACE('',(#1061),#366,.T.);
#5710=ADVANCED_FACE('',(#1062,#532),#5531,.T.);
#5711=ADVANCED_FACE('',(#1063),#367,.T.);
#5712=ADVANCED_FACE('',(#1064),#5532,.T.);
#5713=ADVANCED_FACE('',(#1065),#368,.T.);
#5714=ADVANCED_FACE('',(#1066),#114,.T.);
#5715=ADVANCED_FACE('',(#1067),#369,.T.);
#5716=ADVANCED_FACE('',(#1068),#109,.T.);
#5717=ADVANCED_FACE('',(#1069),#370,.T.);
#5718=ADVANCED_FACE('',(#1070),#5533,.T.);
#5719=ADVANCED_FACE('',(#1071),#5534,.T.);
#5720=ADVANCED_FACE('',(#1072),#128,.F.);
#5721=ADVANCED_FACE('',(#1073),#110,.T.);
#5722=ADVANCED_FACE('',(#1074),#371,.T.);
#5723=ADVANCED_FACE('',(#1075),#115,.T.);
#5724=ADVANCED_FACE('',(#1076),#372,.T.);
#5725=ADVANCED_FACE('',(#1077),#116,.T.);
#5726=ADVANCED_FACE('',(#1078),#373,.T.);
#5727=ADVANCED_FACE('',(#1079),#117,.T.);
#5728=ADVANCED_FACE('',(#1080),#374,.T.);
#5729=ADVANCED_FACE('',(#1081),#5535,.T.);
#5730=ADVANCED_FACE('',(#1082),#375,.T.);
#5731=ADVANCED_FACE('',(#1083),#118,.T.);
#5732=ADVANCED_FACE('',(#1084),#376,.T.);
#5733=ADVANCED_FACE('',(#1085),#119,.T.);
#5734=ADVANCED_FACE('',(#1086),#377,.T.);
#5735=ADVANCED_FACE('',(#1087),#378,.T.);
#5736=ADVANCED_FACE('',(#1088,#533),#5536,.T.);
#5737=ADVANCED_FACE('',(#1089),#379,.T.);
#5738=ADVANCED_FACE('',(#1090),#120,.T.);
#5739=ADVANCED_FACE('',(#1091),#121,.T.);
#5740=ADVANCED_FACE('',(#1092),#380,.T.);
#5741=ADVANCED_FACE('',(#1093),#381,.T.);
#5742=ADVANCED_FACE('',(#1094,#534),#5537,.T.);
#5743=ADVANCED_FACE('',(#1095),#261,.F.);
#5744=ADVANCED_FACE('',(#1096),#382,.F.);
#5745=ADVANCED_FACE('',(#1097),#262,.T.);
#5746=ADVANCED_FACE('',(#1098),#263,.T.);
#5747=ADVANCED_FACE('',(#1099),#129,.T.);
#5748=ADVANCED_FACE('',(#1100),#130,.F.);
#5749=ADVANCED_FACE('',(#1101),#111,.T.);
#5750=ADVANCED_FACE('',(#1102,#535),#5538,.T.);
#5751=ADVANCED_FACE('',(#1103),#383,.F.);
#5752=ADVANCED_FACE('',(#1104),#5539,.F.);
#5753=ADVANCED_FACE('',(#1105),#384,.F.);
#5754=ADVANCED_FACE('',(#1106,#536),#5540,.T.);
#5755=ADVANCED_FACE('',(#1107,#537,#538),#5541,.T.);
#5756=ADVANCED_FACE('',(#1108),#385,.F.);
#5757=ADVANCED_FACE('',(#1109),#386,.F.);
#5758=ADVANCED_FACE('',(#1110,#539),#5542,.T.);
#5759=ADVANCED_FACE('',(#1111),#5543,.T.);
#5760=ADVANCED_FACE('',(#1112),#387,.F.);
#5761=ADVANCED_FACE('',(#1113),#131,.T.);
#5762=ADVANCED_FACE('',(#1114,#540),#5544,.F.);
#5763=ADVANCED_FACE('',(#1115),#388,.F.);
#5764=ADVANCED_FACE('',(#1116),#389,.T.);
#5765=ADVANCED_FACE('',(#1117),#390,.T.);
#5766=ADVANCED_FACE('',(#1118),#5545,.T.);
#5767=ADVANCED_FACE('',(#1119),#5546,.T.);
#5768=ADVANCED_FACE('',(#1120),#5547,.T.);
#5769=ADVANCED_FACE('',(#1121),#5548,.T.);
#5770=ADVANCED_FACE('',(#1122),#391,.T.);
#5771=ADVANCED_FACE('',(#1123),#392,.T.);
#5772=ADVANCED_FACE('',(#1124),#112,.T.);
#5773=ADVANCED_FACE('',(#1125),#113,.T.);
#5774=ADVANCED_FACE('',(#1126),#393,.T.);
#5775=ADVANCED_FACE('',(#1127),#394,.T.);
#5776=ADVANCED_FACE('',(#1128),#132,.T.);
#5777=ADVANCED_FACE('',(#1129),#395,.F.);
#5778=ADVANCED_FACE('',(#1130),#5549,.T.);
#5779=ADVANCED_FACE('',(#1131),#396,.F.);
#5780=ADVANCED_FACE('',(#1132,#541,#542),#5550,.T.);
#5781=ADVANCED_FACE('',(#1133),#397,.F.);
#5782=ADVANCED_FACE('',(#1134),#5551,.T.);
#5783=ADVANCED_FACE('',(#1135),#398,.T.);
#5784=ADVANCED_FACE('',(#1136),#122,.T.);
#5785=ADVANCED_FACE('',(#1137),#399,.T.);
#5786=ADVANCED_FACE('',(#1138),#5552,.T.);
#5787=ADVANCED_FACE('',(#1139),#400,.T.);
#5788=ADVANCED_FACE('',(#1140),#123,.T.);
#5789=ADVANCED_FACE('',(#1141),#401,.T.);
#5790=ADVANCED_FACE('',(#1142),#133,.F.);
#5791=ADVANCED_FACE('',(#1143),#402,.T.);
#5792=ADVANCED_FACE('',(#1144),#403,.T.);
#5793=ADVANCED_FACE('',(#1145),#5553,.T.);
#5794=ADVANCED_FACE('',(#1146),#404,.T.);
#5795=ADVANCED_FACE('',(#1147),#124,.T.);
#5796=ADVANCED_FACE('',(#1148),#405,.T.);
#5797=ADVANCED_FACE('',(#1149),#406,.T.);
#5798=ADVANCED_FACE('',(#1150),#125,.T.);
#5799=ADVANCED_FACE('',(#1151),#407,.T.);
#5800=ADVANCED_FACE('',(#1152),#134,.F.);
#5801=ADVANCED_FACE('',(#1153),#5554,.F.);
#5802=ADVANCED_FACE('',(#1154),#5555,.F.);
#5803=ADVANCED_FACE('',(#1155),#5556,.F.);
#5804=ADVANCED_FACE('',(#1156),#408,.T.);
#5805=ADVANCED_FACE('',(#1157,#543),#5557,.F.);
#5806=ADVANCED_FACE('',(#1158),#409,.T.);
#5807=ADVANCED_FACE('',(#1159,#544),#5558,.F.);
#5808=ADVANCED_FACE('',(#1160,#545),#5559,.F.);
#5809=ADVANCED_FACE('',(#1161),#5560,.T.);
#5810=ADVANCED_FACE('',(#1162),#5561,.T.);
#5811=ADVANCED_FACE('',(#1163),#5562,.T.);
#5812=ADVANCED_FACE('',(#1164),#5563,.T.);
#5813=ADVANCED_FACE('',(#1165),#5564,.T.);
#5814=ADVANCED_FACE('',(#1166),#5565,.T.);
#5815=ADVANCED_FACE('',(#1167,#546),#5566,.T.);
#5816=ADVANCED_FACE('',(#1168),#410,.T.);
#5817=ADVANCED_FACE('',(#1169),#411,.T.);
#5818=ADVANCED_FACE('',(#1170,#547),#5567,.F.);
#5819=ADVANCED_FACE('',(#1171),#412,.F.);
#5820=ADVANCED_FACE('',(#1172,#548),#5568,.T.);
#5821=ADVANCED_FACE('',(#1173),#413,.T.);
#5822=ADVANCED_FACE('',(#1174,#549),#5569,.T.);
#5823=ADVANCED_FACE('',(#1175),#414,.T.);
#5824=ADVANCED_FACE('',(#1176,#550),#5570,.T.);
#5825=ADVANCED_FACE('',(#1177,#551),#5571,.T.);
#5826=ADVANCED_FACE('',(#1178,#552,#553),#415,.T.);
#5827=ADVANCED_FACE('',(#1179,#554,#555,#556,#557,#558,#559,#560,#561,#562),
#5572,.T.);
#5828=ADVANCED_FACE('',(#1180),#416,.F.);
#5829=ADVANCED_FACE('',(#1181,#563),#5573,.T.);
#5830=ADVANCED_FACE('',(#1182),#417,.T.);
#5831=ADVANCED_FACE('',(#1183,#564),#5574,.F.);
#5832=ADVANCED_FACE('',(#1184),#418,.F.);
#5833=ADVANCED_FACE('',(#1185,#565,#566,#567,#568,#569,#570,#571,#572,#573),
#5575,.F.);
#5834=ADVANCED_FACE('',(#1186),#419,.T.);
#5835=ADVANCED_FACE('',(#1187,#574),#5576,.F.);
#5836=ADVANCED_FACE('',(#1188,#575,#576),#420,.F.);
#5837=ADVANCED_FACE('',(#1189),#421,.F.);
#5838=ADVANCED_FACE('',(#1190),#422,.F.);
#5839=ADVANCED_FACE('',(#1191),#423,.F.);
#5840=ADVANCED_FACE('',(#1192),#424,.F.);
#5841=ADVANCED_FACE('',(#1193),#425,.F.);
#5842=ADVANCED_FACE('',(#1194),#426,.F.);
#5843=ADVANCED_FACE('',(#1195),#427,.F.);
#5844=ADVANCED_FACE('',(#1196),#428,.F.);
#5845=ADVANCED_FACE('',(#1197),#429,.F.);
#5846=ADVANCED_FACE('',(#1198),#430,.F.);
#5847=ADVANCED_FACE('',(#1199),#431,.T.);
#5848=ADVANCED_FACE('',(#1200,#577,#578),#5577,.F.);
#5849=ADVANCED_FACE('',(#1201),#432,.F.);
#5850=ADVANCED_FACE('',(#1202,#579),#5578,.T.);
#5851=ADVANCED_FACE('',(#1203),#135,.F.);
#5852=ADVANCED_FACE('',(#1204),#5579,.T.);
#5853=ADVANCED_FACE('',(#1205),#433,.T.);
#5854=ADVANCED_FACE('',(#1206),#136,.T.);
#5855=ADVANCED_FACE('',(#1207),#434,.T.);
#5856=ADVANCED_FACE('',(#1208),#137,.T.);
#5857=ADVANCED_FACE('',(#1209),#435,.T.);
#5858=ADVANCED_FACE('',(#1210),#5580,.T.);
#5859=ADVANCED_FACE('',(#1211),#436,.F.);
#5860=ADVANCED_FACE('',(#1212),#437,.F.);
#5861=ADVANCED_FACE('',(#1213),#438,.T.);
#5862=ADVANCED_FACE('',(#1214,#580),#439,.F.);
#5863=ADVANCED_FACE('',(#1215,#581),#5581,.T.);
#5864=ADVANCED_FACE('',(#1216),#440,.T.);
#5865=ADVANCED_FACE('',(#1217,#582),#5582,.F.);
#5866=ADVANCED_FACE('',(#1218),#5583,.T.);
#5867=ADVANCED_FACE('',(#1219),#441,.T.);
#5868=ADVANCED_FACE('',(#1220,#583),#5584,.T.);
#5869=ADVANCED_FACE('',(#1221),#442,.T.);
#5870=ADVANCED_FACE('',(#1222,#584),#5585,.T.);
#5871=ADVANCED_FACE('',(#1223),#443,.T.);
#5872=ADVANCED_FACE('',(#1224),#5586,.F.);
#5873=ADVANCED_FACE('',(#1225),#5587,.F.);
#5874=ADVANCED_FACE('',(#1226),#5588,.F.);
#5875=ADVANCED_FACE('',(#1227),#5589,.F.);
#5876=ADVANCED_FACE('',(#1228),#5590,.F.);
#5877=ADVANCED_FACE('',(#1229),#444,.T.);
#5878=ADVANCED_FACE('',(#1230,#585),#5591,.T.);
#5879=ADVANCED_FACE('',(#1231),#5592,.F.);
#5880=ADVANCED_FACE('',(#1232,#586,#587),#445,.T.);
#5881=ADVANCED_FACE('',(#1233),#446,.T.);
#5882=ADVANCED_FACE('',(#1234),#447,.T.);
#5883=ADVANCED_FACE('',(#1235),#5593,.T.);
#5884=ADVANCED_FACE('',(#1236),#448,.T.);
#5885=ADVANCED_FACE('',(#1237),#449,.T.);
#5886=ADVANCED_FACE('',(#1238),#5594,.T.);
#5887=ADVANCED_FACE('',(#1239),#5595,.T.);
#5888=ADVANCED_FACE('',(#1240),#5596,.F.);
#5889=ADVANCED_FACE('',(#1241),#5597,.F.);
#5890=ADVANCED_FACE('',(#1242),#5598,.F.);
#5891=ADVANCED_FACE('',(#1243),#450,.T.);
#5892=ADVANCED_FACE('',(#1244,#588,#589),#5599,.T.);
#5893=ADVANCED_FACE('',(#1245),#451,.F.);
#5894=ADVANCED_FACE('',(#1246,#590,#591),#452,.F.);
#5895=ADVANCED_FACE('',(#1247,#592,#593,#594,#595),#5600,.T.);
#5896=ADVANCED_FACE('',(#1248),#453,.T.);
#5897=ADVANCED_FACE('',(#1249),#138,.T.);
#5898=ADVANCED_FACE('',(#1250,#596,#597,#598,#599),#5601,.F.);
#5899=ADVANCED_FACE('',(#1251),#454,.F.);
#5900=ADVANCED_FACE('',(#1252),#455,.F.);
#5901=ADVANCED_FACE('',(#1253),#456,.F.);
#5902=ADVANCED_FACE('',(#1254),#139,.F.);
#5903=ADVANCED_FACE('',(#1255,#600),#457,.T.);
#5904=ADVANCED_FACE('',(#1256),#458,.F.);
#5905=ADVANCED_FACE('',(#1257),#140,.F.);
#5906=ADVANCED_FACE('',(#1258),#5602,.T.);
#5907=ADVANCED_FACE('',(#1259),#5603,.T.);
#5908=ADVANCED_FACE('',(#1260),#141,.T.);
#5909=ADVANCED_FACE('',(#1261),#459,.T.);
#5910=ADVANCED_FACE('',(#1262),#5604,.T.);
#5911=ADVANCED_FACE('',(#1263),#5605,.T.);
#5912=ADVANCED_FACE('',(#1264),#460,.T.);
#5913=ADVANCED_FACE('',(#1265),#5606,.T.);
#5914=ADVANCED_FACE('',(#1266),#461,.T.);
#5915=ADVANCED_FACE('',(#1267,#601),#5607,.F.);
#5916=ADVANCED_FACE('',(#1268),#462,.T.);
#5917=ADVANCED_FACE('',(#1269,#602),#5608,.F.);
#5918=ADVANCED_FACE('',(#1270),#463,.T.);
#5919=ADVANCED_FACE('',(#1271,#603),#5609,.F.);
#5920=ADVANCED_FACE('',(#1272),#464,.T.);
#5921=ADVANCED_FACE('',(#1273,#604),#5610,.F.);
#5922=ADVANCED_FACE('',(#1274),#465,.T.);
#5923=ADVANCED_FACE('',(#1275,#605),#5611,.T.);
#5924=ADVANCED_FACE('',(#1276,#606,#607,#608,#609),#5612,.F.);
#5925=ADVANCED_FACE('',(#1277),#466,.T.);
#5926=ADVANCED_FACE('',(#1278,#610),#5613,.F.);
#5927=ADVANCED_FACE('',(#1279),#467,.F.);
#5928=ADVANCED_FACE('',(#1280,#611),#5614,.T.);
#5929=ADVANCED_FACE('',(#1281),#142,.T.);
#5930=ADVANCED_FACE('',(#1282),#468,.T.);
#5931=ADVANCED_FACE('',(#1283,#612,#613,#614,#615),#5615,.T.);
#5932=ADVANCED_FACE('',(#1284),#469,.F.);
#5933=ADVANCED_FACE('',(#1285),#470,.F.);
#5934=ADVANCED_FACE('',(#1286),#471,.F.);
#5935=ADVANCED_FACE('',(#1287),#143,.T.);
#5936=ADVANCED_FACE('',(#1288),#472,.T.);
#5937=ADVANCED_FACE('',(#1289),#5616,.F.);
#5938=ADVANCED_FACE('',(#1290),#11,.T.);
#5939=ADVANCED_FACE('',(#1291),#12,.T.);
#5940=ADVANCED_FACE('',(#1292),#13,.T.);
#5941=ADVANCED_FACE('',(#1293),#14,.T.);
#5942=ADVANCED_FACE('',(#1294),#15,.T.);
#5943=ADVANCED_FACE('',(#1295),#16,.T.);
#5944=ADVANCED_FACE('',(#1296),#5617,.T.);
#5945=ADVANCED_FACE('',(#1297,#616),#5618,.F.);
#5946=ADVANCED_FACE('',(#1298),#473,.F.);
#5947=ADVANCED_FACE('',(#1299,#617),#5619,.T.);
#5948=ADVANCED_FACE('',(#1300),#5620,.T.);
#5949=ADVANCED_FACE('',(#1301),#5621,.T.);
#5950=ADVANCED_FACE('',(#1302),#5622,.T.);
#5951=ADVANCED_FACE('',(#1303),#5623,.T.);
#5952=ADVANCED_FACE('',(#1304),#5624,.T.);
#5953=ADVANCED_FACE('',(#1305),#5625,.T.);
#5954=ADVANCED_FACE('',(#1306),#474,.T.);
#5955=ADVANCED_FACE('',(#1307,#618),#5626,.F.);
#5956=ADVANCED_FACE('',(#1308),#5627,.T.);
#5957=ADVANCED_FACE('',(#1309),#475,.T.);
#5958=ADVANCED_FACE('',(#1310),#5628,.F.);
#5959=ADVANCED_FACE('',(#1311),#5629,.F.);
#5960=ADVANCED_FACE('',(#1312),#5630,.F.);
#5961=ADVANCED_FACE('',(#1313),#476,.F.);
#5962=ADVANCED_FACE('',(#1314,#619),#5631,.T.);
#5963=ADVANCED_FACE('',(#1315),#477,.T.);
#5964=ADVANCED_FACE('',(#1316),#144,.F.);
#5965=ADVANCED_FACE('',(#1317,#620),#5632,.T.);
#5966=ADVANCED_FACE('',(#1318),#478,.F.);
#5967=ADVANCED_FACE('',(#1319,#621),#5633,.T.);
#5968=ADVANCED_FACE('',(#1320),#145,.F.);
#5969=ADVANCED_FACE('',(#1321),#479,.T.);
#5970=ADVANCED_FACE('',(#1322),#480,.T.);
#5971=ADVANCED_FACE('',(#1323),#481,.T.);
#5972=ADVANCED_FACE('',(#1324),#482,.T.);
#5973=ADVANCED_FACE('',(#1325),#483,.T.);
#5974=ADVANCED_FACE('',(#1326),#484,.T.);
#5975=ADVANCED_FACE('',(#1327,#622),#5634,.F.);
#5976=ADVANCED_FACE('',(#1328,#623),#5635,.F.);
#5977=ADVANCED_FACE('',(#1329),#485,.T.);
#5978=ADVANCED_FACE('',(#1330),#5636,.T.);
#5979=ADVANCED_FACE('',(#1331),#486,.T.);
#5980=ADVANCED_FACE('',(#1332),#5637,.T.);
#5981=ADVANCED_FACE('',(#1333),#487,.T.);
#5982=ADVANCED_FACE('',(#1334,#624),#5638,.T.);
#5983=ADVANCED_FACE('',(#1335),#488,.T.);
#5984=ADVANCED_FACE('',(#1336,#625),#5639,.T.);
#5985=ADVANCED_FACE('',(#1337,#626),#5640,.F.);
#5986=ADVANCED_FACE('',(#1338),#489,.F.);
#5987=ADVANCED_FACE('',(#1339,#627),#5641,.T.);
#5988=ADVANCED_FACE('',(#1340),#490,.T.);
#5989=ADVANCED_FACE('',(#1341,#628),#5642,.F.);
#5990=ADVANCED_FACE('',(#1342),#491,.T.);
#5991=ADVANCED_FACE('',(#1343,#629),#5643,.T.);
#5992=ADVANCED_FACE('',(#1344),#492,.T.);
#5993=ADVANCED_FACE('',(#1345),#493,.T.);
#5994=ADVANCED_FACE('',(#1346,#630),#5644,.F.);
#5995=ADVANCED_FACE('',(#1347,#631,#632),#5645,.F.);
#5996=ADVANCED_FACE('',(#1348),#494,.F.);
#5997=ADVANCED_FACE('',(#1349,#633,#634),#5646,.T.);
#5998=ADVANCED_FACE('',(#1350),#495,.F.);
#5999=ADVANCED_FACE('',(#1351,#635),#5647,.T.);
#6000=ADVANCED_FACE('',(#1352),#496,.T.);
#6001=ADVANCED_FACE('',(#1353),#5648,.T.);
#6002=ADVANCED_FACE('',(#1354),#497,.T.);
#6003=ADVANCED_FACE('',(#1355),#5649,.T.);
#6004=ADVANCED_FACE('',(#1356),#498,.T.);
#6005=ADVANCED_FACE('',(#1357),#5650,.T.);
#6006=ADVANCED_FACE('',(#1358),#499,.T.);
#6007=ADVANCED_FACE('',(#1359),#5651,.T.);
#6008=ADVANCED_FACE('',(#1360),#5652,.F.);
#6009=ADVANCED_FACE('',(#1361),#500,.F.);
#6010=ADVANCED_FACE('',(#1362),#5653,.F.);
#6011=ADVANCED_FACE('',(#1363),#501,.F.);
#6012=ADVANCED_FACE('',(#1364),#5654,.F.);
#6013=ADVANCED_FACE('',(#1365),#502,.F.);
#6014=ADVANCED_FACE('',(#1366),#5655,.F.);
#6015=ADVANCED_FACE('',(#1367),#503,.F.);
#6016=CLOSED_SHELL('',(#5656,#5657,#5658,#5659,#5660,#5661,#5662,#5663,
#5664,#5665,#5666,#5667,#5668,#5669,#5670,#5671,#5672,#5673));
#6017=CLOSED_SHELL('',(#5674,#5675,#5676,#5677,#5678,#5679,#5680,#5681,
#5682,#5683,#5684,#5685,#5686,#5687,#5688,#5689,#5690,#5691,#5692,#5693,
#5694,#5695,#5696,#5697));
#6018=CLOSED_SHELL('',(#5702,#5703,#5704,#5705,#5706,#5707,#5708,#5709,
#5710,#5711,#5712,#5713,#5714,#5715,#5716,#5717,#5718,#5719,#5720,#5721,
#5722,#5723,#5724,#5725,#5726,#5727,#5728,#5729,#5730,#5731,#5732,#5733,
#5734,#5735,#5736,#5737,#5738,#5739,#5740,#5741,#5742,#5743,#5744,#5745,
#5746,#5747,#5748,#5749,#5750,#5751,#5752,#5753,#5754,#5755,#5756,#5757,
#5758,#5759,#5760,#5761,#5762,#5763,#5764,#5765,#5766,#5767,#5768,#5769,
#5770,#5771,#5772,#5773,#5774,#5775,#5776,#5777,#5778,#5779,#5780,#5781,
#5782,#5783,#5784,#5785,#5786,#5787,#5788,#5789,#5790,#5791,#5792,#5793,
#5794,#5795,#5796,#5797,#5798,#5799,#5800,#5801,#5802,#5803));
#6019=CLOSED_SHELL('',(#5808,#5809,#5810,#5811,#5812,#5813,#5814,#5815,
#5816,#5817,#5818,#5819,#5820));
#6020=CLOSED_SHELL('',(#5825,#5826,#5827,#5828,#5829,#5830,#5831,#5832,
#5833,#5834,#5835,#5836,#5837,#5838,#5839,#5840,#5841,#5842,#5843,#5844,
#5845,#5846));
#6021=CLOSED_SHELL('',(#5847,#5848,#5849,#5850,#5851,#5852,#5853,#5854,
#5855,#5856,#5857,#5858,#5859,#5860,#5861,#5862,#5863));
#6022=CLOSED_SHELL('',(#5866,#5867,#5868,#5869,#5870,#5871,#5872,#5873,
#5874,#5875,#5876));
#6023=CLOSED_SHELL('',(#5879,#5880,#5881,#5882,#5883,#5884,#5885,#5886,
#5887,#5888,#5889));
#6024=CLOSED_SHELL('',(#5890,#5891,#5892,#5893,#5894,#5895,#5896,#5897,
#5898,#5899,#5900,#5901,#5902,#5903,#5904,#5905,#5906,#5907,#5908,#5909,
#5910,#5911,#5912,#5913));
#6025=CLOSED_SHELL('',(#5924,#5925,#5926,#5927,#5928,#5929,#5930,#5931,
#5932,#5933,#5934,#5935,#5936));
#6026=CLOSED_SHELL('',(#5937,#5938,#5939,#5940,#5941,#5942,#5943,#5944));
#6027=CLOSED_SHELL('',(#5945,#5946,#5947,#5948,#5949,#5950,#5951,#5952,
#5953));
#6028=CLOSED_SHELL('',(#5956,#5957,#5958,#5959,#5960,#5961,#5962,#5963,
#5964,#5965,#5966,#5967,#5968,#5969,#5970,#5971,#5972,#5973));
#6029=CLOSED_SHELL('',(#5976,#5977,#5978,#5979,#5980));
#6030=CLOSED_SHELL('',(#5985,#5986,#5987,#5988,#5989,#5990,#5991,#5992));
#6031=CLOSED_SHELL('',(#5995,#5996,#5997,#5998,#5999,#6000,#6001,#6002,
#6003,#6004,#6005,#6006,#6007,#6008,#6009,#6010,#6011,#6012,#6013,#6014,
#6015));
#6032=DERIVED_UNIT_ELEMENT(#6064,1.);
#6033=DERIVED_UNIT_ELEMENT(#17115,-3.);
#6034=DERIVED_UNIT_ELEMENT(#6064,1.);
#6035=DERIVED_UNIT_ELEMENT(#17115,-3.);
#6036=DERIVED_UNIT_ELEMENT(#6064,1.);
#6037=DERIVED_UNIT_ELEMENT(#17115,-3.);
#6038=DERIVED_UNIT_ELEMENT(#6064,1.);
#6039=DERIVED_UNIT_ELEMENT(#17115,-3.);
#6040=DERIVED_UNIT_ELEMENT(#6064,1.);
#6041=DERIVED_UNIT_ELEMENT(#17115,-3.);
#6042=DERIVED_UNIT_ELEMENT(#6064,1.);
#6043=DERIVED_UNIT_ELEMENT(#17115,-3.);
#6044=DERIVED_UNIT_ELEMENT(#6064,1.);
#6045=DERIVED_UNIT_ELEMENT(#17115,-3.);
#6046=DERIVED_UNIT_ELEMENT(#6064,1.);
#6047=DERIVED_UNIT_ELEMENT(#17115,-3.);
#6048=DERIVED_UNIT_ELEMENT(#6064,1.);
#6049=DERIVED_UNIT_ELEMENT(#17115,-3.);
#6050=DERIVED_UNIT_ELEMENT(#6064,1.);
#6051=DERIVED_UNIT_ELEMENT(#17115,-3.);
#6052=DERIVED_UNIT_ELEMENT(#6064,1.);
#6053=DERIVED_UNIT_ELEMENT(#17115,-3.);
#6054=DERIVED_UNIT_ELEMENT(#6064,1.);
#6055=DERIVED_UNIT_ELEMENT(#17115,-3.);
#6056=DERIVED_UNIT_ELEMENT(#6064,1.);
#6057=DERIVED_UNIT_ELEMENT(#17115,-3.);
#6058=DERIVED_UNIT_ELEMENT(#6064,1.);
#6059=DERIVED_UNIT_ELEMENT(#17115,-3.);
#6060=DERIVED_UNIT_ELEMENT(#6064,1.);
#6061=DERIVED_UNIT_ELEMENT(#17115,-3.);
#6062=DERIVED_UNIT_ELEMENT(#6064,1.);
#6063=DERIVED_UNIT_ELEMENT(#17115,-3.);
#6064=(
MASS_UNIT()
NAMED_UNIT(*)
SI_UNIT(.KILO.,.GRAM.)
);
#6065=DERIVED_UNIT((#6032,#6033));
#6066=DERIVED_UNIT((#6034,#6035));
#6067=DERIVED_UNIT((#6036,#6037));
#6068=DERIVED_UNIT((#6038,#6039));
#6069=DERIVED_UNIT((#6040,#6041));
#6070=DERIVED_UNIT((#6042,#6043));
#6071=DERIVED_UNIT((#6044,#6045));
#6072=DERIVED_UNIT((#6046,#6047));
#6073=DERIVED_UNIT((#6048,#6049));
#6074=DERIVED_UNIT((#6050,#6051));
#6075=DERIVED_UNIT((#6052,#6053));
#6076=DERIVED_UNIT((#6054,#6055));
#6077=DERIVED_UNIT((#6056,#6057));
#6078=DERIVED_UNIT((#6058,#6059));
#6079=DERIVED_UNIT((#6060,#6061));
#6080=DERIVED_UNIT((#6062,#6063));
#6081=MEASURE_REPRESENTATION_ITEM('density measure',
POSITIVE_RATIO_MEASURE(7850.),#6065);
#6082=MEASURE_REPRESENTATION_ITEM('density measure',
POSITIVE_RATIO_MEASURE(7850.),#6066);
#6083=MEASURE_REPRESENTATION_ITEM('density measure',
POSITIVE_RATIO_MEASURE(7850.),#6067);
#6084=MEASURE_REPRESENTATION_ITEM('density measure',
POSITIVE_RATIO_MEASURE(7850.),#6068);
#6085=MEASURE_REPRESENTATION_ITEM('density measure',
POSITIVE_RATIO_MEASURE(7850.),#6069);
#6086=MEASURE_REPRESENTATION_ITEM('density measure',
POSITIVE_RATIO_MEASURE(7850.),#6070);
#6087=MEASURE_REPRESENTATION_ITEM('density measure',
POSITIVE_RATIO_MEASURE(7850.),#6071);
#6088=MEASURE_REPRESENTATION_ITEM('density measure',
POSITIVE_RATIO_MEASURE(7850.),#6072);
#6089=MEASURE_REPRESENTATION_ITEM('density measure',
POSITIVE_RATIO_MEASURE(7850.),#6073);
#6090=MEASURE_REPRESENTATION_ITEM('density measure',
POSITIVE_RATIO_MEASURE(7850.),#6074);
#6091=MEASURE_REPRESENTATION_ITEM('density measure',
POSITIVE_RATIO_MEASURE(7850.),#6075);
#6092=MEASURE_REPRESENTATION_ITEM('density measure',
POSITIVE_RATIO_MEASURE(7850.),#6076);
#6093=MEASURE_REPRESENTATION_ITEM('density measure',
POSITIVE_RATIO_MEASURE(7850.),#6077);
#6094=MEASURE_REPRESENTATION_ITEM('density measure',
POSITIVE_RATIO_MEASURE(7850.),#6078);
#6095=MEASURE_REPRESENTATION_ITEM('density measure',
POSITIVE_RATIO_MEASURE(7850.),#6079);
#6096=MEASURE_REPRESENTATION_ITEM('density measure',
POSITIVE_RATIO_MEASURE(7850.),#6080);
#6097=PROPERTY_DEFINITION_REPRESENTATION(#6177,#6129);
#6098=PROPERTY_DEFINITION_REPRESENTATION(#6178,#6130);
#6099=PROPERTY_DEFINITION_REPRESENTATION(#6179,#6131);
#6100=PROPERTY_DEFINITION_REPRESENTATION(#6180,#6132);
#6101=PROPERTY_DEFINITION_REPRESENTATION(#6181,#6133);
#6102=PROPERTY_DEFINITION_REPRESENTATION(#6182,#6134);
#6103=PROPERTY_DEFINITION_REPRESENTATION(#6183,#6135);
#6104=PROPERTY_DEFINITION_REPRESENTATION(#6184,#6136);
#6105=PROPERTY_DEFINITION_REPRESENTATION(#6185,#6137);
#6106=PROPERTY_DEFINITION_REPRESENTATION(#6186,#6138);
#6107=PROPERTY_DEFINITION_REPRESENTATION(#6187,#6139);
#6108=PROPERTY_DEFINITION_REPRESENTATION(#6188,#6140);
#6109=PROPERTY_DEFINITION_REPRESENTATION(#6189,#6141);
#6110=PROPERTY_DEFINITION_REPRESENTATION(#6190,#6142);
#6111=PROPERTY_DEFINITION_REPRESENTATION(#6191,#6143);
#6112=PROPERTY_DEFINITION_REPRESENTATION(#6192,#6144);
#6113=PROPERTY_DEFINITION_REPRESENTATION(#6193,#6145);
#6114=PROPERTY_DEFINITION_REPRESENTATION(#6194,#6146);
#6115=PROPERTY_DEFINITION_REPRESENTATION(#6195,#6147);
#6116=PROPERTY_DEFINITION_REPRESENTATION(#6196,#6148);
#6117=PROPERTY_DEFINITION_REPRESENTATION(#6197,#6149);
#6118=PROPERTY_DEFINITION_REPRESENTATION(#6198,#6150);
#6119=PROPERTY_DEFINITION_REPRESENTATION(#6199,#6151);
#6120=PROPERTY_DEFINITION_REPRESENTATION(#6200,#6152);
#6121=PROPERTY_DEFINITION_REPRESENTATION(#6201,#6153);
#6122=PROPERTY_DEFINITION_REPRESENTATION(#6202,#6154);
#6123=PROPERTY_DEFINITION_REPRESENTATION(#6203,#6155);
#6124=PROPERTY_DEFINITION_REPRESENTATION(#6204,#6156);
#6125=PROPERTY_DEFINITION_REPRESENTATION(#6205,#6157);
#6126=PROPERTY_DEFINITION_REPRESENTATION(#6206,#6158);
#6127=PROPERTY_DEFINITION_REPRESENTATION(#6207,#6159);
#6128=PROPERTY_DEFINITION_REPRESENTATION(#6208,#6160);
#6129=REPRESENTATION('material name',(#6161),#17092);
#6130=REPRESENTATION('density',(#6081),#17092);
#6131=REPRESENTATION('material name',(#6162),#17094);
#6132=REPRESENTATION('density',(#6082),#17094);
#6133=REPRESENTATION('material name',(#6163),#17095);
#6134=REPRESENTATION('density',(#6083),#17095);
#6135=REPRESENTATION('material name',(#6164),#17096);
#6136=REPRESENTATION('density',(#6084),#17096);
#6137=REPRESENTATION('material name',(#6165),#17098);
#6138=REPRESENTATION('density',(#6085),#17098);
#6139=REPRESENTATION('material name',(#6166),#17100);
#6140=REPRESENTATION('density',(#6086),#17100);
#6141=REPRESENTATION('material name',(#6167),#17101);
#6142=REPRESENTATION('density',(#6087),#17101);
#6143=REPRESENTATION('material name',(#6168),#17102);
#6144=REPRESENTATION('density',(#6088),#17102);
#6145=REPRESENTATION('material name',(#6169),#17104);
#6146=REPRESENTATION('density',(#6089),#17104);
#6147=REPRESENTATION('material name',(#6170),#17105);
#6148=REPRESENTATION('density',(#6090),#17105);
#6149=REPRESENTATION('material name',(#6171),#17106);
#6150=REPRESENTATION('density',(#6091),#17106);
#6151=REPRESENTATION('material name',(#6172),#17107);
#6152=REPRESENTATION('density',(#6092),#17107);
#6153=REPRESENTATION('material name',(#6173),#17109);
#6154=REPRESENTATION('density',(#6093),#17109);
#6155=REPRESENTATION('material name',(#6174),#17110);
#6156=REPRESENTATION('density',(#6094),#17110);
#6157=REPRESENTATION('material name',(#6175),#17111);
#6158=REPRESENTATION('density',(#6095),#17111);
#6159=REPRESENTATION('material name',(#6176),#17112);
#6160=REPRESENTATION('density',(#6096),#17112);
#6161=DESCRIPTIVE_REPRESENTATION_ITEM('Steel','Steel');
#6162=DESCRIPTIVE_REPRESENTATION_ITEM('Steel','Steel');
#6163=DESCRIPTIVE_REPRESENTATION_ITEM('Steel','Steel');
#6164=DESCRIPTIVE_REPRESENTATION_ITEM('Steel','Steel');
#6165=DESCRIPTIVE_REPRESENTATION_ITEM('Steel','Steel');
#6166=DESCRIPTIVE_REPRESENTATION_ITEM('Steel','Steel');
#6167=DESCRIPTIVE_REPRESENTATION_ITEM('Steel','Steel');
#6168=DESCRIPTIVE_REPRESENTATION_ITEM('Steel','Steel');
#6169=DESCRIPTIVE_REPRESENTATION_ITEM('Steel','Steel');
#6170=DESCRIPTIVE_REPRESENTATION_ITEM('Steel','Steel');
#6171=DESCRIPTIVE_REPRESENTATION_ITEM('Steel','Steel');
#6172=DESCRIPTIVE_REPRESENTATION_ITEM('Steel','Steel');
#6173=DESCRIPTIVE_REPRESENTATION_ITEM('Steel','Steel');
#6174=DESCRIPTIVE_REPRESENTATION_ITEM('Steel','Steel');
#6175=DESCRIPTIVE_REPRESENTATION_ITEM('Steel','Steel');
#6176=DESCRIPTIVE_REPRESENTATION_ITEM('Steel','Steel');
#6177=PROPERTY_DEFINITION('material property','material name',#17208);
#6178=PROPERTY_DEFINITION('material property','density of part',#17208);
#6179=PROPERTY_DEFINITION('material property','material name',#17210);
#6180=PROPERTY_DEFINITION('material property','density of part',#17210);
#6181=PROPERTY_DEFINITION('material property','material name',#17211);
#6182=PROPERTY_DEFINITION('material property','density of part',#17211);
#6183=PROPERTY_DEFINITION('material property','material name',#17212);
#6184=PROPERTY_DEFINITION('material property','density of part',#17212);
#6185=PROPERTY_DEFINITION('material property','material name',#17214);
#6186=PROPERTY_DEFINITION('material property','density of part',#17214);
#6187=PROPERTY_DEFINITION('material property','material name',#17216);
#6188=PROPERTY_DEFINITION('material property','density of part',#17216);
#6189=PROPERTY_DEFINITION('material property','material name',#17217);
#6190=PROPERTY_DEFINITION('material property','density of part',#17217);
#6191=PROPERTY_DEFINITION('material property','material name',#17218);
#6192=PROPERTY_DEFINITION('material property','density of part',#17218);
#6193=PROPERTY_DEFINITION('material property','material name',#17220);
#6194=PROPERTY_DEFINITION('material property','density of part',#17220);
#6195=PROPERTY_DEFINITION('material property','material name',#17221);
#6196=PROPERTY_DEFINITION('material property','density of part',#17221);
#6197=PROPERTY_DEFINITION('material property','material name',#17222);
#6198=PROPERTY_DEFINITION('material property','density of part',#17222);
#6199=PROPERTY_DEFINITION('material property','material name',#17223);
#6200=PROPERTY_DEFINITION('material property','density of part',#17223);
#6201=PROPERTY_DEFINITION('material property','material name',#17225);
#6202=PROPERTY_DEFINITION('material property','density of part',#17225);
#6203=PROPERTY_DEFINITION('material property','material name',#17226);
#6204=PROPERTY_DEFINITION('material property','density of part',#17226);
#6205=PROPERTY_DEFINITION('material property','material name',#17227);
#6206=PROPERTY_DEFINITION('material property','density of part',#17227);
#6207=PROPERTY_DEFINITION('material property','material name',#17228);
#6208=PROPERTY_DEFINITION('material property','density of part',#17228);
#6209=AXIS2_PLACEMENT_3D('',#8877,#6978,#6979);
#6210=AXIS2_PLACEMENT_3D('',#8878,#6980,#6981);
#6211=AXIS2_PLACEMENT_3D('',#8879,#6982,#6983);
#6212=AXIS2_PLACEMENT_3D('',#8888,#6988,#6989);
#6213=AXIS2_PLACEMENT_3D('',#8894,#6993,#6994);
#6214=AXIS2_PLACEMENT_3D('',#8900,#6998,#6999);
#6215=AXIS2_PLACEMENT_3D('',#8911,#7005,#7006);
#6216=AXIS2_PLACEMENT_3D('',#8913,#7007,#7008);
#6217=AXIS2_PLACEMENT_3D('',#8914,#7009,#7010);
#6218=AXIS2_PLACEMENT_3D('',#8920,#7014,#7015);
#6219=AXIS2_PLACEMENT_3D('',#8922,#7017,#7018);
#6220=AXIS2_PLACEMENT_3D('',#8925,#7020,#7021);
#6221=AXIS2_PLACEMENT_3D('',#8927,#7022,#7023);
#6222=AXIS2_PLACEMENT_3D('',#8929,#7024,#7025);
#6223=AXIS2_PLACEMENT_3D('',#8931,#7026,#7027);
#6224=AXIS2_PLACEMENT_3D('',#8932,#7028,#7029);
#6225=AXIS2_PLACEMENT_3D('',#8934,#7031,#7032);
#6226=AXIS2_PLACEMENT_3D('',#8936,#7034,#7035);
#6227=AXIS2_PLACEMENT_3D('',#8938,#7036,#7037);
#6228=AXIS2_PLACEMENT_3D('',#8940,#7038,#7039);
#6229=AXIS2_PLACEMENT_3D('',#8942,#7040,#7041);
#6230=AXIS2_PLACEMENT_3D('',#8944,#7042,#7043);
#6231=AXIS2_PLACEMENT_3D('',#8945,#7044,#7045);
#6232=AXIS2_PLACEMENT_3D('',#8947,#7047,#7048);
#6233=AXIS2_PLACEMENT_3D('',#8949,#7050,#7051);
#6234=AXIS2_PLACEMENT_3D('',#8951,#7053,#7054);
#6235=AXIS2_PLACEMENT_3D('',#8953,#7056,#7057);
#6236=AXIS2_PLACEMENT_3D('',#8955,#7058,#7059);
#6237=AXIS2_PLACEMENT_3D('',#8957,#7061,#7062);
#6238=AXIS2_PLACEMENT_3D('',#8958,#7063,#7064);
#6239=AXIS2_PLACEMENT_3D('',#8960,#7065,#7066);
#6240=AXIS2_PLACEMENT_3D('',#8961,#7067,#7068);
#6241=AXIS2_PLACEMENT_3D('',#8963,#7070,#7071);
#6242=AXIS2_PLACEMENT_3D('',#8964,#7072,#7073);
#6243=AXIS2_PLACEMENT_3D('',#8965,#7074,#7075);
#6244=AXIS2_PLACEMENT_3D('',#8968,#7076,#7077);
#6245=AXIS2_PLACEMENT_3D('',#8972,#7079,#7080);
#6246=AXIS2_PLACEMENT_3D('',#8976,#7082,#7083);
#6247=AXIS2_PLACEMENT_3D('',#8980,#7085,#7086);
#6248=AXIS2_PLACEMENT_3D('',#8983,#7088,#7089);
#6249=AXIS2_PLACEMENT_3D('',#8985,#7090,#7091);
#6250=AXIS2_PLACEMENT_3D('',#8987,#7092,#7093);
#6251=AXIS2_PLACEMENT_3D('',#8989,#7094,#7095);
#6252=AXIS2_PLACEMENT_3D('',#8991,#7096,#7097);
#6253=AXIS2_PLACEMENT_3D('',#8993,#7098,#7099);
#6254=AXIS2_PLACEMENT_3D('',#8994,#7100,#7101);
#6255=AXIS2_PLACEMENT_3D('',#8997,#7103,#7104);
#6256=AXIS2_PLACEMENT_3D('',#8998,#7105,#7106);
#6257=AXIS2_PLACEMENT_3D('',#9001,#7107,#7108);
#6258=AXIS2_PLACEMENT_3D('',#9005,#7110,#7111);
#6259=AXIS2_PLACEMENT_3D('',#9009,#7113,#7114);
#6260=AXIS2_PLACEMENT_3D('',#9013,#7116,#7117);
#6261=AXIS2_PLACEMENT_3D('',#9016,#7119,#7120);
#6262=AXIS2_PLACEMENT_3D('',#9018,#7121,#7122);
#6263=AXIS2_PLACEMENT_3D('',#9020,#7123,#7124);
#6264=AXIS2_PLACEMENT_3D('',#9022,#7125,#7126);
#6265=AXIS2_PLACEMENT_3D('',#9024,#7127,#7128);
#6266=AXIS2_PLACEMENT_3D('',#9025,#7129,#7130);
#6267=AXIS2_PLACEMENT_3D('',#9027,#7132,#7133);
#6268=AXIS2_PLACEMENT_3D('',#9029,#7135,#7136);
#6269=AXIS2_PLACEMENT_3D('',#9031,#7138,#7139);
#6270=AXIS2_PLACEMENT_3D('',#9033,#7141,#7142);
#6271=AXIS2_PLACEMENT_3D('',#9035,#7144,#7145);
#6272=AXIS2_PLACEMENT_3D('',#9039,#7147,#7148);
#6273=AXIS2_PLACEMENT_3D('',#9041,#7150,#7151);
#6274=AXIS2_PLACEMENT_3D('',#9045,#7154,#7155);
#6275=AXIS2_PLACEMENT_3D('',#9047,#7156,#7157);
#6276=AXIS2_PLACEMENT_3D('',#9049,#7159,#7160);
#6277=AXIS2_PLACEMENT_3D('',#9053,#7163,#7164);
#6278=AXIS2_PLACEMENT_3D('',#9055,#7165,#7166);
#6279=AXIS2_PLACEMENT_3D('',#9057,#7168,#7169);
#6280=AXIS2_PLACEMENT_3D('',#9061,#7172,#7173);
#6281=AXIS2_PLACEMENT_3D('',#9063,#7174,#7175);
#6282=AXIS2_PLACEMENT_3D('',#9065,#7177,#7178);
#6283=AXIS2_PLACEMENT_3D('',#9067,#7180,#7181);
#6284=AXIS2_PLACEMENT_3D('',#9070,#7184,#7185);
#6285=AXIS2_PLACEMENT_3D('',#9072,#7187,#7188);
#6286=AXIS2_PLACEMENT_3D('',#9074,#7190,#7191);
#6287=AXIS2_PLACEMENT_3D('',#9076,#7193,#7194);
#6288=AXIS2_PLACEMENT_3D('',#9078,#7196,#7197);
#6289=AXIS2_PLACEMENT_3D('',#9080,#7199,#7200);
#6290=AXIS2_PLACEMENT_3D('',#9082,#7202,#7203);
#6291=AXIS2_PLACEMENT_3D('',#9083,#7204,#7205);
#6292=AXIS2_PLACEMENT_3D('',#9085,#7206,#7207);
#6293=AXIS2_PLACEMENT_3D('',#9088,#7209,#7210);
#6294=AXIS2_PLACEMENT_3D('',#9089,#7211,#7212);
#6295=AXIS2_PLACEMENT_3D('',#9091,#7213,#7214);
#6296=AXIS2_PLACEMENT_3D('',#9092,#7215,#7216);
#6297=AXIS2_PLACEMENT_3D('',#9094,#7217,#7218);
#6298=AXIS2_PLACEMENT_3D('',#9097,#7220,#7221);
#6299=AXIS2_PLACEMENT_3D('',#9098,#7222,#7223);
#6300=AXIS2_PLACEMENT_3D('',#9100,#7224,#7225);
#6301=AXIS2_PLACEMENT_3D('',#9101,#7226,#7227);
#6302=AXIS2_PLACEMENT_3D('',#9102,#7228,#7229);
#6303=AXIS2_PLACEMENT_3D('',#9126,#7235,#7236);
#6304=AXIS2_PLACEMENT_3D('',#9127,#7237,#7238);
#6305=AXIS2_PLACEMENT_3D('',#9131,#7240,#7241);
#6306=AXIS2_PLACEMENT_3D('',#9132,#7242,#7243);
#6307=AXIS2_PLACEMENT_3D('',#9133,#7244,#7245);
#6308=AXIS2_PLACEMENT_3D('',#9135,#7246,#7247);
#6309=AXIS2_PLACEMENT_3D('',#9136,#7248,#7249);
#6310=AXIS2_PLACEMENT_3D('',#9137,#7250,#7251);
#6311=AXIS2_PLACEMENT_3D('',#9139,#7252,#7253);
#6312=AXIS2_PLACEMENT_3D('',#9140,#7254,#7255);
#6313=AXIS2_PLACEMENT_3D('',#9143,#7257,#7258);
#6314=AXIS2_PLACEMENT_3D('',#9182,#7259,#7260);
#6315=AXIS2_PLACEMENT_3D('',#9184,#7261,#7262);
#6316=AXIS2_PLACEMENT_3D('',#9185,#7263,#7264);
#6317=AXIS2_PLACEMENT_3D('',#9187,#7265,#7266);
#6318=AXIS2_PLACEMENT_3D('',#9189,#7267,#7268);
#6319=AXIS2_PLACEMENT_3D('',#9190,#7269,#7270);
#6320=AXIS2_PLACEMENT_3D('',#9191,#7271,#7272);
#6321=AXIS2_PLACEMENT_3D('',#9194,#7274,#7275);
#6322=AXIS2_PLACEMENT_3D('',#9195,#7276,#7277);
#6323=AXIS2_PLACEMENT_3D('',#9218,#7283,#7284);
#6324=AXIS2_PLACEMENT_3D('',#9222,#7286,#7287);
#6325=AXIS2_PLACEMENT_3D('',#9223,#7288,#7289);
#6326=AXIS2_PLACEMENT_3D('',#9224,#7290,#7291);
#6327=AXIS2_PLACEMENT_3D('',#9230,#7295,#7296);
#6328=AXIS2_PLACEMENT_3D('',#9232,#7297,#7298);
#6329=AXIS2_PLACEMENT_3D('',#9235,#7300,#7301);
#6330=AXIS2_PLACEMENT_3D('',#9236,#7302,#7303);
#6331=AXIS2_PLACEMENT_3D('',#9237,#7304,#7305);
#6332=AXIS2_PLACEMENT_3D('',#9238,#7306,#7307);
#6333=AXIS2_PLACEMENT_3D('',#9239,#7308,#7309);
#6334=AXIS2_PLACEMENT_3D('',#9242,#7311,#7312);
#6335=AXIS2_PLACEMENT_3D('',#9345,#7313,#7314);
#6336=AXIS2_PLACEMENT_3D('',#9346,#7315,#7316);
#6337=AXIS2_PLACEMENT_3D('',#9349,#7318,#7319);
#6338=AXIS2_PLACEMENT_3D('',#9350,#7320,#7321);
#6339=AXIS2_PLACEMENT_3D('',#9354,#7323,#7324);
#6340=AXIS2_PLACEMENT_3D('',#9355,#7325,#7326);
#6341=AXIS2_PLACEMENT_3D('',#9356,#7327,#7328);
#6342=AXIS2_PLACEMENT_3D('',#9358,#7329,#7330);
#6343=AXIS2_PLACEMENT_3D('',#9362,#7333,#7334);
#6344=AXIS2_PLACEMENT_3D('',#9364,#7335,#7336);
#6345=AXIS2_PLACEMENT_3D('',#9366,#7337,#7338);
#6346=AXIS2_PLACEMENT_3D('',#9367,#7339,#7340);
#6347=AXIS2_PLACEMENT_3D('',#9475,#7341,#7342);
#6348=AXIS2_PLACEMENT_3D('',#9476,#7343,#7344);
#6349=AXIS2_PLACEMENT_3D('',#9477,#7345,#7346);
#6350=AXIS2_PLACEMENT_3D('',#9478,#7347,#7348);
#6351=AXIS2_PLACEMENT_3D('',#9479,#7349,#7350);
#6352=AXIS2_PLACEMENT_3D('',#9480,#7351,#7352);
#6353=AXIS2_PLACEMENT_3D('',#9481,#7353,#7354);
#6354=AXIS2_PLACEMENT_3D('',#9482,#7355,#7356);
#6355=AXIS2_PLACEMENT_3D('',#9484,#7357,#7358);
#6356=AXIS2_PLACEMENT_3D('',#9485,#7359,#7360);
#6357=AXIS2_PLACEMENT_3D('',#9486,#7361,#7362);
#6358=AXIS2_PLACEMENT_3D('',#9489,#7364,#7365);
#6359=AXIS2_PLACEMENT_3D('',#9490,#7366,#7367);
#6360=AXIS2_PLACEMENT_3D('',#9491,#7368,#7369);
#6361=AXIS2_PLACEMENT_3D('',#9492,#7370,#7371);
#6362=AXIS2_PLACEMENT_3D('',#9495,#7373,#7374);
#6363=AXIS2_PLACEMENT_3D('',#9496,#7375,#7376);
#6364=AXIS2_PLACEMENT_3D('',#9500,#7379,#7380);
#6365=AXIS2_PLACEMENT_3D('',#9502,#7381,#7382);
#6366=AXIS2_PLACEMENT_3D('',#9505,#7384,#7385);
#6367=AXIS2_PLACEMENT_3D('',#9506,#7386,#7387);
#6368=AXIS2_PLACEMENT_3D('',#9507,#7388,#7389);
#6369=AXIS2_PLACEMENT_3D('',#9508,#7390,#7391);
#6370=AXIS2_PLACEMENT_3D('',#9511,#7393,#7394);
#6371=AXIS2_PLACEMENT_3D('',#9512,#7395,#7396);
#6372=AXIS2_PLACEMENT_3D('',#9513,#7397,#7398);
#6373=AXIS2_PLACEMENT_3D('',#9514,#7399,#7400);
#6374=AXIS2_PLACEMENT_3D('',#9515,#7401,#7402);
#6375=AXIS2_PLACEMENT_3D('',#9516,#7403,#7404);
#6376=AXIS2_PLACEMENT_3D('',#9519,#7406,#7407);
#6377=AXIS2_PLACEMENT_3D('',#9520,#7408,#7409);
#6378=AXIS2_PLACEMENT_3D('',#9523,#7411,#7412);
#6379=AXIS2_PLACEMENT_3D('',#9524,#7413,#7414);
#6380=AXIS2_PLACEMENT_3D('',#9525,#7415,#7416);
#6381=AXIS2_PLACEMENT_3D('',#9526,#7417,#7418);
#6382=AXIS2_PLACEMENT_3D('',#9527,#7419,#7420);
#6383=AXIS2_PLACEMENT_3D('',#9528,#7421,#7422);
#6384=AXIS2_PLACEMENT_3D('',#9529,#7423,#7424);
#6385=AXIS2_PLACEMENT_3D('',#9530,#7425,#7426);
#6386=AXIS2_PLACEMENT_3D('',#9531,#7427,#7428);
#6387=AXIS2_PLACEMENT_3D('',#9533,#7429,#7430);
#6388=AXIS2_PLACEMENT_3D('',#9535,#7432,#7433);
#6389=AXIS2_PLACEMENT_3D('',#9537,#7434,#7435);
#6390=AXIS2_PLACEMENT_3D('',#9538,#7436,#7437);
#6391=AXIS2_PLACEMENT_3D('',#9540,#7438,#7439);
#6392=AXIS2_PLACEMENT_3D('',#9542,#7441,#7442);
#6393=AXIS2_PLACEMENT_3D('',#9544,#7444,#7445);
#6394=AXIS2_PLACEMENT_3D('',#9547,#7446,#7447);
#6395=AXIS2_PLACEMENT_3D('',#9549,#7449,#7450);
#6396=AXIS2_PLACEMENT_3D('',#9550,#7451,#7452);
#6397=AXIS2_PLACEMENT_3D('',#9553,#7453,#7454);
#6398=AXIS2_PLACEMENT_3D('',#9554,#7455,#7456);
#6399=AXIS2_PLACEMENT_3D('',#9558,#7458,#7459);
#6400=AXIS2_PLACEMENT_3D('',#9559,#7460,#7461);
#6401=AXIS2_PLACEMENT_3D('',#9560,#7462,#7463);
#6402=AXIS2_PLACEMENT_3D('',#9561,#7464,#7465);
#6403=AXIS2_PLACEMENT_3D('',#9562,#7466,#7467);
#6404=AXIS2_PLACEMENT_3D('',#9564,#7468,#7469);
#6405=AXIS2_PLACEMENT_3D('',#9577,#7470,#7471);
#6406=AXIS2_PLACEMENT_3D('',#9670,#7472,#7473);
#6407=AXIS2_PLACEMENT_3D('',#9692,#7474,#7475);
#6408=AXIS2_PLACEMENT_3D('',#9777,#7476,#7477);
#6409=AXIS2_PLACEMENT_3D('',#9876,#7478,#7479);
#6410=AXIS2_PLACEMENT_3D('',#9877,#7480,#7481);
#6411=AXIS2_PLACEMENT_3D('',#9878,#7482,#7483);
#6412=AXIS2_PLACEMENT_3D('',#9888,#7488,#7489);
#6413=AXIS2_PLACEMENT_3D('',#9899,#7495,#7496);
#6414=AXIS2_PLACEMENT_3D('',#9900,#7497,#7498);
#6415=AXIS2_PLACEMENT_3D('',#9936,#7501,#7502);
#6416=AXIS2_PLACEMENT_3D('',#9955,#7503,#7504);
#6417=AXIS2_PLACEMENT_3D('',#9956,#7505,#7506);
#6418=AXIS2_PLACEMENT_3D('',#9959,#7508,#7509);
#6419=AXIS2_PLACEMENT_3D('',#9960,#7510,#7511);
#6420=AXIS2_PLACEMENT_3D('',#9962,#7512,#7513);
#6421=AXIS2_PLACEMENT_3D('',#9968,#7516,#7517);
#6422=AXIS2_PLACEMENT_3D('',#9972,#7520,#7521);
#6423=AXIS2_PLACEMENT_3D('',#9973,#7522,#7523);
#6424=AXIS2_PLACEMENT_3D('',#10002,#7531,#7532);
#6425=AXIS2_PLACEMENT_3D('',#10003,#7533,#7534);
#6426=AXIS2_PLACEMENT_3D('',#10058,#7536,#7537);
#6427=AXIS2_PLACEMENT_3D('',#10060,#7538,#7539);
#6428=AXIS2_PLACEMENT_3D('',#10064,#7542,#7543);
#6429=AXIS2_PLACEMENT_3D('',#10065,#7544,#7545);
#6430=AXIS2_PLACEMENT_3D('',#10101,#7553,#7554);
#6431=AXIS2_PLACEMENT_3D('',#10102,#7555,#7556);
#6432=AXIS2_PLACEMENT_3D('',#10103,#7557,#7558);
#6433=AXIS2_PLACEMENT_3D('',#10105,#7559,#7560);
#6434=AXIS2_PLACEMENT_3D('',#10110,#7563,#7564);
#6435=AXIS2_PLACEMENT_3D('',#10111,#7565,#7566);
#6436=AXIS2_PLACEMENT_3D('',#10114,#7567,#7568);
#6437=AXIS2_PLACEMENT_3D('',#10115,#7569,#7570);
#6438=AXIS2_PLACEMENT_3D('',#10116,#7571,#7572);
#6439=AXIS2_PLACEMENT_3D('',#10117,#7573,#7574);
#6440=AXIS2_PLACEMENT_3D('',#10135,#7584,#7585);
#6441=AXIS2_PLACEMENT_3D('',#10137,#7586,#7587);
#6442=AXIS2_PLACEMENT_3D('',#10138,#7588,#7589);
#6443=AXIS2_PLACEMENT_3D('',#10140,#7591,#7592);
#6444=AXIS2_PLACEMENT_3D('',#10141,#7593,#7594);
#6445=AXIS2_PLACEMENT_3D('',#10142,#7595,#7596);
#6446=AXIS2_PLACEMENT_3D('',#10143,#7597,#7598);
#6447=AXIS2_PLACEMENT_3D('',#10145,#7600,#7601);
#6448=AXIS2_PLACEMENT_3D('',#10147,#7603,#7604);
#6449=AXIS2_PLACEMENT_3D('',#10148,#7605,#7606);
#6450=AXIS2_PLACEMENT_3D('',#10150,#7608,#7609);
#6451=AXIS2_PLACEMENT_3D('',#10152,#7611,#7612);
#6452=AXIS2_PLACEMENT_3D('',#10153,#7613,#7614);
#6453=AXIS2_PLACEMENT_3D('',#10154,#7615,#7616);
#6454=AXIS2_PLACEMENT_3D('',#10199,#7617,#7618);
#6455=AXIS2_PLACEMENT_3D('',#10252,#7619,#7620);
#6456=AXIS2_PLACEMENT_3D('',#10253,#7621,#7622);
#6457=AXIS2_PLACEMENT_3D('',#10254,#7623,#7624);
#6458=AXIS2_PLACEMENT_3D('',#10255,#7625,#7626);
#6459=AXIS2_PLACEMENT_3D('',#10256,#7627,#7628);
#6460=AXIS2_PLACEMENT_3D('',#10258,#7629,#7630);
#6461=AXIS2_PLACEMENT_3D('',#10259,#7631,#7632);
#6462=AXIS2_PLACEMENT_3D('',#10260,#7633,#7634);
#6463=AXIS2_PLACEMENT_3D('',#10265,#7637,#7638);
#6464=AXIS2_PLACEMENT_3D('',#10266,#7639,#7640);
#6465=AXIS2_PLACEMENT_3D('',#10268,#7641,#7642);
#6466=AXIS2_PLACEMENT_3D('',#10274,#7646,#7647);
#6467=AXIS2_PLACEMENT_3D('',#10275,#7648,#7649);
#6468=AXIS2_PLACEMENT_3D('',#10277,#7650,#7651);
#6469=AXIS2_PLACEMENT_3D('',#10279,#7653,#7654);
#6470=AXIS2_PLACEMENT_3D('',#10281,#7655,#7656);
#6471=AXIS2_PLACEMENT_3D('',#10284,#7658,#7659);
#6472=AXIS2_PLACEMENT_3D('',#10286,#7660,#7661);
#6473=AXIS2_PLACEMENT_3D('',#10289,#7663,#7664);
#6474=AXIS2_PLACEMENT_3D('',#10291,#7665,#7666);
#6475=AXIS2_PLACEMENT_3D('',#10292,#7667,#7668);
#6476=AXIS2_PLACEMENT_3D('',#10294,#7670,#7671);
#6477=AXIS2_PLACEMENT_3D('',#10295,#7672,#7673);
#6478=AXIS2_PLACEMENT_3D('',#10301,#7677,#7678);
#6479=AXIS2_PLACEMENT_3D('',#10302,#7679,#7680);
#6480=AXIS2_PLACEMENT_3D('',#10303,#7681,#7682);
#6481=AXIS2_PLACEMENT_3D('',#10305,#7683,#7684);
#6482=AXIS2_PLACEMENT_3D('',#10306,#7685,#7686);
#6483=AXIS2_PLACEMENT_3D('',#10307,#7687,#7688);
#6484=AXIS2_PLACEMENT_3D('',#10309,#7690,#7691);
#6485=AXIS2_PLACEMENT_3D('',#10313,#7694,#7695);
#6486=AXIS2_PLACEMENT_3D('',#10314,#7696,#7697);
#6487=AXIS2_PLACEMENT_3D('',#10315,#7698,#7699);
#6488=AXIS2_PLACEMENT_3D('',#10316,#7700,#7701);
#6489=AXIS2_PLACEMENT_3D('',#10317,#7702,#7703);
#6490=AXIS2_PLACEMENT_3D('',#10318,#7704,#7705);
#6491=AXIS2_PLACEMENT_3D('',#10319,#7706,#7707);
#6492=AXIS2_PLACEMENT_3D('',#10320,#7708,#7709);
#6493=AXIS2_PLACEMENT_3D('',#10321,#7710,#7711);
#6494=AXIS2_PLACEMENT_3D('',#10322,#7712,#7713);
#6495=AXIS2_PLACEMENT_3D('',#10324,#7714,#7715);
#6496=AXIS2_PLACEMENT_3D('',#10326,#7717,#7718);
#6497=AXIS2_PLACEMENT_3D('',#10330,#7721,#7722);
#6498=AXIS2_PLACEMENT_3D('',#10331,#7723,#7724);
#6499=AXIS2_PLACEMENT_3D('',#10332,#7725,#7726);
#6500=AXIS2_PLACEMENT_3D('',#10333,#7727,#7728);
#6501=AXIS2_PLACEMENT_3D('',#10334,#7729,#7730);
#6502=AXIS2_PLACEMENT_3D('',#10335,#7731,#7732);
#6503=AXIS2_PLACEMENT_3D('',#10336,#7733,#7734);
#6504=AXIS2_PLACEMENT_3D('',#10337,#7735,#7736);
#6505=AXIS2_PLACEMENT_3D('',#10338,#7737,#7738);
#6506=AXIS2_PLACEMENT_3D('',#10339,#7739,#7740);
#6507=AXIS2_PLACEMENT_3D('',#10340,#7741,#7742);
#6508=AXIS2_PLACEMENT_3D('',#10341,#7743,#7744);
#6509=AXIS2_PLACEMENT_3D('',#10342,#7745,#7746);
#6510=AXIS2_PLACEMENT_3D('',#10343,#7747,#7748);
#6511=AXIS2_PLACEMENT_3D('',#10345,#7750,#7751);
#6512=AXIS2_PLACEMENT_3D('',#10347,#7753,#7754);
#6513=AXIS2_PLACEMENT_3D('',#10348,#7755,#7756);
#6514=AXIS2_PLACEMENT_3D('',#10350,#7757,#7758);
#6515=AXIS2_PLACEMENT_3D('',#10353,#7760,#7761);
#6516=AXIS2_PLACEMENT_3D('',#10354,#7762,#7763);
#6517=AXIS2_PLACEMENT_3D('',#10356,#7764,#7765);
#6518=AXIS2_PLACEMENT_3D('',#10357,#7766,#7767);
#6519=AXIS2_PLACEMENT_3D('',#10359,#7768,#7769);
#6520=AXIS2_PLACEMENT_3D('',#10362,#7771,#7772);
#6521=AXIS2_PLACEMENT_3D('',#10363,#7773,#7774);
#6522=AXIS2_PLACEMENT_3D('',#10365,#7775,#7776);
#6523=AXIS2_PLACEMENT_3D('',#10366,#7777,#7778);
#6524=AXIS2_PLACEMENT_3D('',#10367,#7779,#7780);
#6525=AXIS2_PLACEMENT_3D('',#10381,#7787,#7788);
#6526=AXIS2_PLACEMENT_3D('',#10382,#7789,#7790);
#6527=AXIS2_PLACEMENT_3D('',#10388,#7794,#7795);
#6528=AXIS2_PLACEMENT_3D('',#10392,#7798,#7799);
#6529=AXIS2_PLACEMENT_3D('',#10396,#7802,#7803);
#6530=AXIS2_PLACEMENT_3D('',#10400,#7806,#7807);
#6531=AXIS2_PLACEMENT_3D('',#10404,#7810,#7811);
#6532=AXIS2_PLACEMENT_3D('',#10406,#7813,#7814);
#6533=AXIS2_PLACEMENT_3D('',#10408,#7815,#7816);
#6534=AXIS2_PLACEMENT_3D('',#10409,#7817,#7818);
#6535=AXIS2_PLACEMENT_3D('',#10412,#7820,#7821);
#6536=AXIS2_PLACEMENT_3D('',#10413,#7822,#7823);
#6537=AXIS2_PLACEMENT_3D('',#10415,#7824,#7825);
#6538=AXIS2_PLACEMENT_3D('',#10417,#7827,#7828);
#6539=AXIS2_PLACEMENT_3D('',#10419,#7829,#7830);
#6540=AXIS2_PLACEMENT_3D('',#10420,#7831,#7832);
#6541=AXIS2_PLACEMENT_3D('',#10423,#7834,#7835);
#6542=AXIS2_PLACEMENT_3D('',#10424,#7836,#7837);
#6543=AXIS2_PLACEMENT_3D('',#10425,#7838,#7839);
#6544=AXIS2_PLACEMENT_3D('',#10427,#7840,#7841);
#6545=AXIS2_PLACEMENT_3D('',#10430,#7843,#7844);
#6546=AXIS2_PLACEMENT_3D('',#10431,#7845,#7846);
#6547=AXIS2_PLACEMENT_3D('',#10433,#7847,#7848);
#6548=AXIS2_PLACEMENT_3D('',#10434,#7849,#7850);
#6549=AXIS2_PLACEMENT_3D('',#10436,#7851,#7852);
#6550=AXIS2_PLACEMENT_3D('',#10439,#7854,#7855);
#6551=AXIS2_PLACEMENT_3D('',#10440,#7856,#7857);
#6552=AXIS2_PLACEMENT_3D('',#10442,#7858,#7859);
#6553=AXIS2_PLACEMENT_3D('',#10443,#7860,#7861);
#6554=AXIS2_PLACEMENT_3D('',#10444,#7862,#7863);
#6555=AXIS2_PLACEMENT_3D('',#10445,#7864,#7865);
#6556=AXIS2_PLACEMENT_3D('',#10446,#7866,#7867);
#6557=AXIS2_PLACEMENT_3D('',#10447,#7868,#7869);
#6558=AXIS2_PLACEMENT_3D('',#10448,#7870,#7871);
#6559=AXIS2_PLACEMENT_3D('',#10449,#7872,#7873);
#6560=AXIS2_PLACEMENT_3D('',#10451,#7874,#7875);
#6561=AXIS2_PLACEMENT_3D('',#10453,#7876,#7877);
#6562=AXIS2_PLACEMENT_3D('',#10454,#7878,#7879);
#6563=AXIS2_PLACEMENT_3D('',#10457,#7881,#7882);
#6564=AXIS2_PLACEMENT_3D('',#10532,#7883,#7884);
#6565=AXIS2_PLACEMENT_3D('',#10534,#7885,#7886);
#6566=AXIS2_PLACEMENT_3D('',#10536,#7887,#7888);
#6567=AXIS2_PLACEMENT_3D('',#10538,#7889,#7890);
#6568=AXIS2_PLACEMENT_3D('',#10540,#7891,#7892);
#6569=AXIS2_PLACEMENT_3D('',#10542,#7893,#7894);
#6570=AXIS2_PLACEMENT_3D('',#10544,#7895,#7896);
#6571=AXIS2_PLACEMENT_3D('',#10546,#7897,#7898);
#6572=AXIS2_PLACEMENT_3D('',#10548,#7899,#7900);
#6573=AXIS2_PLACEMENT_3D('',#10550,#7901,#7902);
#6574=AXIS2_PLACEMENT_3D('',#10551,#7903,#7904);
#6575=AXIS2_PLACEMENT_3D('',#10554,#7906,#7907);
#6576=AXIS2_PLACEMENT_3D('',#10555,#7908,#7909);
#6577=AXIS2_PLACEMENT_3D('',#10557,#7910,#7911);
#6578=AXIS2_PLACEMENT_3D('',#10558,#7912,#7913);
#6579=AXIS2_PLACEMENT_3D('',#10561,#7915,#7916);
#6580=AXIS2_PLACEMENT_3D('',#10562,#7917,#7918);
#6581=AXIS2_PLACEMENT_3D('',#10564,#7919,#7920);
#6582=AXIS2_PLACEMENT_3D('',#10565,#7921,#7922);
#6583=AXIS2_PLACEMENT_3D('',#10568,#7924,#7925);
#6584=AXIS2_PLACEMENT_3D('',#10569,#7926,#7927);
#6585=AXIS2_PLACEMENT_3D('',#10571,#7928,#7929);
#6586=AXIS2_PLACEMENT_3D('',#10573,#7930,#7931);
#6587=AXIS2_PLACEMENT_3D('',#10575,#7932,#7933);
#6588=AXIS2_PLACEMENT_3D('',#10577,#7934,#7935);
#6589=AXIS2_PLACEMENT_3D('',#10579,#7936,#7937);
#6590=AXIS2_PLACEMENT_3D('',#10581,#7938,#7939);
#6591=AXIS2_PLACEMENT_3D('',#10583,#7940,#7941);
#6592=AXIS2_PLACEMENT_3D('',#10585,#7942,#7943);
#6593=AXIS2_PLACEMENT_3D('',#10587,#7944,#7945);
#6594=AXIS2_PLACEMENT_3D('',#10588,#7946,#7947);
#6595=AXIS2_PLACEMENT_3D('',#10591,#7949,#7950);
#6596=AXIS2_PLACEMENT_3D('',#10592,#7951,#7952);
#6597=AXIS2_PLACEMENT_3D('',#10594,#7953,#7954);
#6598=AXIS2_PLACEMENT_3D('',#10595,#7955,#7956);
#6599=AXIS2_PLACEMENT_3D('',#10671,#7958,#7959);
#6600=AXIS2_PLACEMENT_3D('',#10673,#7961,#7962);
#6601=AXIS2_PLACEMENT_3D('',#10675,#7964,#7965);
#6602=AXIS2_PLACEMENT_3D('',#10677,#7967,#7968);
#6603=AXIS2_PLACEMENT_3D('',#10679,#7970,#7971);
#6604=AXIS2_PLACEMENT_3D('',#10681,#7973,#7974);
#6605=AXIS2_PLACEMENT_3D('',#10683,#7976,#7977);
#6606=AXIS2_PLACEMENT_3D('',#10685,#7979,#7980);
#6607=AXIS2_PLACEMENT_3D('',#10687,#7982,#7983);
#6608=AXIS2_PLACEMENT_3D('',#10689,#7985,#7986);
#6609=AXIS2_PLACEMENT_3D('',#10691,#7988,#7989);
#6610=AXIS2_PLACEMENT_3D('',#10692,#7990,#7991);
#6611=AXIS2_PLACEMENT_3D('',#10693,#7992,#7993);
#6612=AXIS2_PLACEMENT_3D('',#10695,#7994,#7995);
#6613=AXIS2_PLACEMENT_3D('',#10710,#7997,#7998);
#6614=AXIS2_PLACEMENT_3D('',#10749,#8000,#8001);
#6615=AXIS2_PLACEMENT_3D('',#10771,#8003,#8004);
#6616=AXIS2_PLACEMENT_3D('',#10774,#8005,#8006);
#6617=AXIS2_PLACEMENT_3D('',#10778,#8008,#8009);
#6618=AXIS2_PLACEMENT_3D('',#10781,#8011,#8012);
#6619=AXIS2_PLACEMENT_3D('',#10783,#8013,#8014);
#6620=AXIS2_PLACEMENT_3D('',#10784,#8015,#8016);
#6621=AXIS2_PLACEMENT_3D('',#10787,#8018,#8019);
#6622=AXIS2_PLACEMENT_3D('',#10788,#8020,#8021);
#6623=AXIS2_PLACEMENT_3D('',#10791,#8022,#8023);
#6624=AXIS2_PLACEMENT_3D('',#10795,#8025,#8026);
#6625=AXIS2_PLACEMENT_3D('',#10797,#8028,#8029);
#6626=AXIS2_PLACEMENT_3D('',#10820,#8030,#8031);
#6627=AXIS2_PLACEMENT_3D('',#10826,#8034,#8035);
#6628=AXIS2_PLACEMENT_3D('',#10828,#8037,#8038);
#6629=AXIS2_PLACEMENT_3D('',#10829,#8039,#8040);
#6630=AXIS2_PLACEMENT_3D('',#10830,#8041,#8042);
#6631=AXIS2_PLACEMENT_3D('',#10831,#8043,#8044);
#6632=AXIS2_PLACEMENT_3D('',#10832,#8045,#8046);
#6633=AXIS2_PLACEMENT_3D('',#10833,#8047,#8048);
#6634=AXIS2_PLACEMENT_3D('',#10834,#8049,#8050);
#6635=AXIS2_PLACEMENT_3D('',#10837,#8052,#8053);
#6636=AXIS2_PLACEMENT_3D('',#10838,#8054,#8055);
#6637=AXIS2_PLACEMENT_3D('',#10839,#8056,#8057);
#6638=AXIS2_PLACEMENT_3D('',#10840,#8058,#8059);
#6639=AXIS2_PLACEMENT_3D('',#10842,#8061,#8062);
#6640=AXIS2_PLACEMENT_3D('',#10843,#8063,#8064);
#6641=AXIS2_PLACEMENT_3D('',#10844,#8065,#8066);
#6642=AXIS2_PLACEMENT_3D('',#10891,#8068,#8069);
#6643=AXIS2_PLACEMENT_3D('',#10932,#8071,#8072);
#6644=AXIS2_PLACEMENT_3D('',#10933,#8073,#8074);
#6645=AXIS2_PLACEMENT_3D('',#10937,#8077,#8078);
#6646=AXIS2_PLACEMENT_3D('',#10938,#8079,#8080);
#6647=AXIS2_PLACEMENT_3D('',#10939,#8081,#8082);
#6648=AXIS2_PLACEMENT_3D('',#10941,#8083,#8084);
#6649=AXIS2_PLACEMENT_3D('',#10944,#8086,#8087);
#6650=AXIS2_PLACEMENT_3D('',#10945,#8088,#8089);
#6651=AXIS2_PLACEMENT_3D('',#10947,#8090,#8091);
#6652=AXIS2_PLACEMENT_3D('',#10948,#8092,#8093);
#6653=AXIS2_PLACEMENT_3D('',#10949,#8094,#8095);
#6654=AXIS2_PLACEMENT_3D('',#10951,#8096,#8097);
#6655=AXIS2_PLACEMENT_3D('',#10952,#8098,#8099);
#6656=AXIS2_PLACEMENT_3D('',#10955,#8101,#8102);
#6657=AXIS2_PLACEMENT_3D('',#10956,#8103,#8104);
#6658=AXIS2_PLACEMENT_3D('',#10958,#8105,#8106);
#6659=AXIS2_PLACEMENT_3D('',#10959,#8107,#8108);
#6660=AXIS2_PLACEMENT_3D('',#10962,#8110,#8111);
#6661=AXIS2_PLACEMENT_3D('',#10963,#8112,#8113);
#6662=AXIS2_PLACEMENT_3D('',#10965,#8114,#8115);
#6663=AXIS2_PLACEMENT_3D('',#10966,#8116,#8117);
#6664=AXIS2_PLACEMENT_3D('',#10970,#8119,#8120);
#6665=AXIS2_PLACEMENT_3D('',#10974,#8122,#8123);
#6666=AXIS2_PLACEMENT_3D('',#10978,#8125,#8126);
#6667=AXIS2_PLACEMENT_3D('',#10982,#8128,#8129);
#6668=AXIS2_PLACEMENT_3D('',#10985,#8131,#8132);
#6669=AXIS2_PLACEMENT_3D('',#10986,#8133,#8134);
#6670=AXIS2_PLACEMENT_3D('',#10989,#8137,#8138);
#6671=AXIS2_PLACEMENT_3D('',#10991,#8140,#8141);
#6672=AXIS2_PLACEMENT_3D('',#10993,#8143,#8144);
#6673=AXIS2_PLACEMENT_3D('',#10994,#8145,#8146);
#6674=AXIS2_PLACEMENT_3D('',#10995,#8147,#8148);
#6675=AXIS2_PLACEMENT_3D('',#10997,#8149,#8150);
#6676=AXIS2_PLACEMENT_3D('',#11000,#8152,#8153);
#6677=AXIS2_PLACEMENT_3D('',#11001,#8154,#8155);
#6678=AXIS2_PLACEMENT_3D('',#11003,#8156,#8157);
#6679=AXIS2_PLACEMENT_3D('',#11004,#8158,#8159);
#6680=AXIS2_PLACEMENT_3D('',#11005,#8160,#8161);
#6681=AXIS2_PLACEMENT_3D('',#11007,#8162,#8163);
#6682=AXIS2_PLACEMENT_3D('',#11008,#8164,#8165);
#6683=AXIS2_PLACEMENT_3D('',#11010,#8166,#8167);
#6684=AXIS2_PLACEMENT_3D('',#11166,#8171,#8172);
#6685=AXIS2_PLACEMENT_3D('',#11168,#8173,#8174);
#6686=AXIS2_PLACEMENT_3D('',#11170,#8176,#8177);
#6687=AXIS2_PLACEMENT_3D('',#11173,#8179,#8180);
#6688=AXIS2_PLACEMENT_3D('',#11174,#8181,#8182);
#6689=AXIS2_PLACEMENT_3D('',#11175,#8183,#8184);
#6690=AXIS2_PLACEMENT_3D('',#11178,#8186,#8187);
#6691=AXIS2_PLACEMENT_3D('',#11179,#8188,#8189);
#6692=AXIS2_PLACEMENT_3D('',#11181,#8190,#8191);
#6693=AXIS2_PLACEMENT_3D('',#11183,#8193,#8194);
#6694=AXIS2_PLACEMENT_3D('',#11184,#8195,#8196);
#6695=AXIS2_PLACEMENT_3D('',#11185,#8197,#8198);
#6696=AXIS2_PLACEMENT_3D('',#11186,#8199,#8200);
#6697=AXIS2_PLACEMENT_3D('',#11187,#8201,#8202);
#6698=AXIS2_PLACEMENT_3D('',#11188,#8203,#8204);
#6699=AXIS2_PLACEMENT_3D('',#11189,#8205,#8206);
#6700=AXIS2_PLACEMENT_3D('',#11190,#8207,#8208);
#6701=AXIS2_PLACEMENT_3D('',#11191,#8209,#8210);
#6702=AXIS2_PLACEMENT_3D('',#11192,#8211,#8212);
#6703=AXIS2_PLACEMENT_3D('',#11193,#8213,#8214);
#6704=AXIS2_PLACEMENT_3D('',#11194,#8215,#8216);
#6705=AXIS2_PLACEMENT_3D('',#11202,#8220,#8221);
#6706=AXIS2_PLACEMENT_3D('',#11203,#8222,#8223);
#6707=AXIS2_PLACEMENT_3D('',#11205,#8224,#8225);
#6708=AXIS2_PLACEMENT_3D('',#11207,#8226,#8227);
#6709=AXIS2_PLACEMENT_3D('',#11209,#8229,#8230);
#6710=AXIS2_PLACEMENT_3D('',#11216,#8234,#8235);
#6711=AXIS2_PLACEMENT_3D('',#11218,#8236,#8237);
#6712=AXIS2_PLACEMENT_3D('',#11220,#8238,#8239);
#6713=AXIS2_PLACEMENT_3D('',#11221,#8240,#8241);
#6714=AXIS2_PLACEMENT_3D('',#11261,#8243,#8244);
#6715=AXIS2_PLACEMENT_3D('',#11263,#8245,#8246);
#6716=AXIS2_PLACEMENT_3D('',#11266,#8248,#8249);
#6717=AXIS2_PLACEMENT_3D('',#11305,#8250,#8251);
#6718=AXIS2_PLACEMENT_3D('',#11307,#8252,#8253);
#6719=AXIS2_PLACEMENT_3D('',#11309,#8254,#8255);
#6720=AXIS2_PLACEMENT_3D('',#11311,#8256,#8257);
#6721=AXIS2_PLACEMENT_3D('',#11313,#8258,#8259);
#6722=AXIS2_PLACEMENT_3D('',#11314,#8260,#8261);
#6723=AXIS2_PLACEMENT_3D('',#11318,#8263,#8264);
#6724=AXIS2_PLACEMENT_3D('',#11319,#8265,#8266);
#6725=AXIS2_PLACEMENT_3D('',#11320,#8267,#8268);
#6726=AXIS2_PLACEMENT_3D('',#11322,#8269,#8270);
#6727=AXIS2_PLACEMENT_3D('',#11323,#8271,#8272);
#6728=AXIS2_PLACEMENT_3D('',#11324,#8273,#8274);
#6729=AXIS2_PLACEMENT_3D('',#11326,#8275,#8276);
#6730=AXIS2_PLACEMENT_3D('',#11328,#8277,#8278);
#6731=AXIS2_PLACEMENT_3D('',#11330,#8279,#8280);
#6732=AXIS2_PLACEMENT_3D('',#11332,#8281,#8282);
#6733=AXIS2_PLACEMENT_3D('',#11333,#8283,#8284);
#6734=AXIS2_PLACEMENT_3D('',#11335,#8286,#8287);
#6735=AXIS2_PLACEMENT_3D('',#11337,#8289,#8290);
#6736=AXIS2_PLACEMENT_3D('',#11339,#8292,#8293);
#6737=AXIS2_PLACEMENT_3D('',#11341,#8294,#8295);
#6738=AXIS2_PLACEMENT_3D('',#11343,#8296,#8297);
#6739=AXIS2_PLACEMENT_3D('',#11344,#8298,#8299);
#6740=AXIS2_PLACEMENT_3D('',#11345,#8300,#8301);
#6741=AXIS2_PLACEMENT_3D('',#11349,#8303,#8304);
#6742=AXIS2_PLACEMENT_3D('',#11352,#8306,#8307);
#6743=AXIS2_PLACEMENT_3D('',#11389,#8309,#8310);
#6744=AXIS2_PLACEMENT_3D('',#11391,#8312,#8313);
#6745=AXIS2_PLACEMENT_3D('',#11394,#8314,#8315);
#6746=AXIS2_PLACEMENT_3D('',#11403,#8316,#8317);
#6747=AXIS2_PLACEMENT_3D('',#11406,#8320,#8321);
#6748=AXIS2_PLACEMENT_3D('',#11407,#8322,#8323);
#6749=AXIS2_PLACEMENT_3D('',#11408,#8324,#8325);
#6750=AXIS2_PLACEMENT_3D('',#11409,#8326,#8327);
#6751=AXIS2_PLACEMENT_3D('',#11411,#8329,#8330);
#6752=AXIS2_PLACEMENT_3D('',#11412,#8331,#8332);
#6753=AXIS2_PLACEMENT_3D('',#11413,#8333,#8334);
#6754=AXIS2_PLACEMENT_3D('',#11415,#8335,#8336);
#6755=AXIS2_PLACEMENT_3D('',#11417,#8338,#8339);
#6756=AXIS2_PLACEMENT_3D('',#11418,#8340,#8341);
#6757=AXIS2_PLACEMENT_3D('',#11420,#8342,#8343);
#6758=AXIS2_PLACEMENT_3D('',#11423,#8345,#8346);
#6759=AXIS2_PLACEMENT_3D('',#11424,#8347,#8348);
#6760=AXIS2_PLACEMENT_3D('',#11426,#8349,#8350);
#6761=AXIS2_PLACEMENT_3D('',#11427,#8351,#8352);
#6762=AXIS2_PLACEMENT_3D('',#11429,#8353,#8354);
#6763=AXIS2_PLACEMENT_3D('',#11432,#8356,#8357);
#6764=AXIS2_PLACEMENT_3D('',#11433,#8358,#8359);
#6765=AXIS2_PLACEMENT_3D('',#11435,#8360,#8361);
#6766=AXIS2_PLACEMENT_3D('',#11436,#8362,#8363);
#6767=AXIS2_PLACEMENT_3D('',#11438,#8364,#8365);
#6768=AXIS2_PLACEMENT_3D('',#11441,#8367,#8368);
#6769=AXIS2_PLACEMENT_3D('',#11442,#8369,#8370);
#6770=AXIS2_PLACEMENT_3D('',#11444,#8371,#8372);
#6771=AXIS2_PLACEMENT_3D('',#11445,#8373,#8374);
#6772=AXIS2_PLACEMENT_3D('',#11447,#8375,#8376);
#6773=AXIS2_PLACEMENT_3D('',#11450,#8378,#8379);
#6774=AXIS2_PLACEMENT_3D('',#11451,#8380,#8381);
#6775=AXIS2_PLACEMENT_3D('',#11453,#8382,#8383);
#6776=AXIS2_PLACEMENT_3D('',#11454,#8384,#8385);
#6777=AXIS2_PLACEMENT_3D('',#11456,#8386,#8387);
#6778=AXIS2_PLACEMENT_3D('',#11459,#8389,#8390);
#6779=AXIS2_PLACEMENT_3D('',#11460,#8391,#8392);
#6780=AXIS2_PLACEMENT_3D('',#11462,#8393,#8394);
#6781=AXIS2_PLACEMENT_3D('',#11463,#8395,#8396);
#6782=AXIS2_PLACEMENT_3D('',#11464,#8397,#8398);
#6783=AXIS2_PLACEMENT_3D('',#11466,#8399,#8400);
#6784=AXIS2_PLACEMENT_3D('',#11468,#8401,#8402);
#6785=AXIS2_PLACEMENT_3D('',#11470,#8403,#8404);
#6786=AXIS2_PLACEMENT_3D('',#11472,#8405,#8406);
#6787=AXIS2_PLACEMENT_3D('',#11474,#8407,#8408);
#6788=AXIS2_PLACEMENT_3D('',#11475,#8409,#8410);
#6789=AXIS2_PLACEMENT_3D('',#11478,#8412,#8413);
#6790=AXIS2_PLACEMENT_3D('',#11479,#8414,#8415);
#6791=AXIS2_PLACEMENT_3D('',#11481,#8416,#8417);
#6792=AXIS2_PLACEMENT_3D('',#11482,#8418,#8419);
#6793=AXIS2_PLACEMENT_3D('',#11485,#8421,#8422);
#6794=AXIS2_PLACEMENT_3D('',#11486,#8423,#8424);
#6795=AXIS2_PLACEMENT_3D('',#11488,#8425,#8426);
#6796=AXIS2_PLACEMENT_3D('',#11489,#8427,#8428);
#6797=AXIS2_PLACEMENT_3D('',#11491,#8429,#8430);
#6798=AXIS2_PLACEMENT_3D('',#11493,#8431,#8432);
#6799=AXIS2_PLACEMENT_3D('',#11494,#8433,#8434);
#6800=AXIS2_PLACEMENT_3D('',#11495,#8435,#8436);
#6801=AXIS2_PLACEMENT_3D('',#11498,#8438,#8439);
#6802=AXIS2_PLACEMENT_3D('',#11499,#8440,#8441);
#6803=AXIS2_PLACEMENT_3D('',#11501,#8442,#8443);
#6804=AXIS2_PLACEMENT_3D('',#11503,#8444,#8445);
#6805=AXIS2_PLACEMENT_3D('',#11505,#8446,#8447);
#6806=AXIS2_PLACEMENT_3D('',#11507,#8448,#8449);
#6807=AXIS2_PLACEMENT_3D('',#11508,#8450,#8451);
#6808=AXIS2_PLACEMENT_3D('',#11510,#8453,#8454);
#6809=AXIS2_PLACEMENT_3D('',#11512,#8456,#8457);
#6810=AXIS2_PLACEMENT_3D('',#11514,#8459,#8460);
#6811=AXIS2_PLACEMENT_3D('',#11516,#8461,#8462);
#6812=AXIS2_PLACEMENT_3D('',#11518,#8463,#8464);
#6813=AXIS2_PLACEMENT_3D('',#11519,#8465,#8466);
#6814=AXIS2_PLACEMENT_3D('',#11520,#8467,#8468);
#6815=AXIS2_PLACEMENT_3D('',#11522,#8470,#8471);
#6816=AXIS2_PLACEMENT_3D('',#11523,#8472,#8473);
#6817=AXIS2_PLACEMENT_3D('',#16706,#8474,#8475);
#6818=AXIS2_PLACEMENT_3D('',#16707,#8476,#8477);
#6819=AXIS2_PLACEMENT_3D('',#16708,#8478,#8479);
#6820=AXIS2_PLACEMENT_3D('',#16722,#8486,#8487);
#6821=AXIS2_PLACEMENT_3D('',#16723,#8488,#8489);
#6822=AXIS2_PLACEMENT_3D('',#16726,#8491,#8492);
#6823=AXIS2_PLACEMENT_3D('',#16727,#8493,#8494);
#6824=AXIS2_PLACEMENT_3D('',#16740,#8501,#8502);
#6825=AXIS2_PLACEMENT_3D('',#16743,#8505,#8506);
#6826=AXIS2_PLACEMENT_3D('',#16745,#8508,#8509);
#6827=AXIS2_PLACEMENT_3D('',#16747,#8511,#8512);
#6828=AXIS2_PLACEMENT_3D('',#16749,#8514,#8515);
#6829=AXIS2_PLACEMENT_3D('',#16751,#8517,#8518);
#6830=AXIS2_PLACEMENT_3D('',#16752,#8519,#8520);
#6831=AXIS2_PLACEMENT_3D('',#16754,#8521,#8522);
#6832=AXIS2_PLACEMENT_3D('',#16757,#8524,#8525);
#6833=AXIS2_PLACEMENT_3D('',#16758,#8526,#8527);
#6834=AXIS2_PLACEMENT_3D('',#16760,#8528,#8529);
#6835=AXIS2_PLACEMENT_3D('',#16761,#8530,#8531);
#6836=AXIS2_PLACEMENT_3D('',#16762,#8532,#8533);
#6837=AXIS2_PLACEMENT_3D('',#16763,#8534,#8535);
#6838=AXIS2_PLACEMENT_3D('',#16766,#8536,#8537);
#6839=AXIS2_PLACEMENT_3D('',#16768,#8538,#8539);
#6840=AXIS2_PLACEMENT_3D('',#16770,#8540,#8541);
#6841=AXIS2_PLACEMENT_3D('',#16774,#8543,#8544);
#6842=AXIS2_PLACEMENT_3D('',#16776,#8545,#8546);
#6843=AXIS2_PLACEMENT_3D('',#16778,#8547,#8548);
#6844=AXIS2_PLACEMENT_3D('',#16780,#8550,#8551);
#6845=AXIS2_PLACEMENT_3D('',#16783,#8552,#8553);
#6846=AXIS2_PLACEMENT_3D('',#16786,#8556,#8557);
#6847=AXIS2_PLACEMENT_3D('',#16788,#8558,#8559);
#6848=AXIS2_PLACEMENT_3D('',#16789,#8560,#8561);
#6849=AXIS2_PLACEMENT_3D('',#16793,#8563,#8564);
#6850=AXIS2_PLACEMENT_3D('',#16797,#8566,#8567);
#6851=AXIS2_PLACEMENT_3D('',#16798,#8568,#8569);
#6852=AXIS2_PLACEMENT_3D('',#16799,#8570,#8571);
#6853=AXIS2_PLACEMENT_3D('',#16802,#8572,#8573);
#6854=AXIS2_PLACEMENT_3D('',#16806,#8575,#8576);
#6855=AXIS2_PLACEMENT_3D('',#16810,#8578,#8579);
#6856=AXIS2_PLACEMENT_3D('',#16811,#8580,#8581);
#6857=AXIS2_PLACEMENT_3D('',#16812,#8582,#8583);
#6858=AXIS2_PLACEMENT_3D('',#16815,#8585,#8586);
#6859=AXIS2_PLACEMENT_3D('',#16816,#8587,#8588);
#6860=AXIS2_PLACEMENT_3D('',#16818,#8589,#8590);
#6861=AXIS2_PLACEMENT_3D('',#16819,#8591,#8592);
#6862=AXIS2_PLACEMENT_3D('',#16823,#8594,#8595);
#6863=AXIS2_PLACEMENT_3D('',#16824,#8596,#8597);
#6864=AXIS2_PLACEMENT_3D('',#16825,#8598,#8599);
#6865=AXIS2_PLACEMENT_3D('',#16834,#8600,#8601);
#6866=AXIS2_PLACEMENT_3D('',#16842,#8604,#8605);
#6867=AXIS2_PLACEMENT_3D('',#16843,#8606,#8607);
#6868=AXIS2_PLACEMENT_3D('',#16846,#8609,#8610);
#6869=AXIS2_PLACEMENT_3D('',#16847,#8611,#8612);
#6870=AXIS2_PLACEMENT_3D('',#16853,#8614,#8615);
#6871=AXIS2_PLACEMENT_3D('',#16854,#8616,#8617);
#6872=AXIS2_PLACEMENT_3D('',#16856,#8619,#8620);
#6873=AXIS2_PLACEMENT_3D('',#16858,#8622,#8623);
#6874=AXIS2_PLACEMENT_3D('',#16859,#8624,#8625);
#6875=AXIS2_PLACEMENT_3D('',#16861,#8627,#8628);
#6876=AXIS2_PLACEMENT_3D('',#16862,#8629,#8630);
#6877=AXIS2_PLACEMENT_3D('',#16864,#8631,#8632);
#6878=AXIS2_PLACEMENT_3D('',#16867,#8634,#8635);
#6879=AXIS2_PLACEMENT_3D('',#16868,#8636,#8637);
#6880=AXIS2_PLACEMENT_3D('',#16870,#8638,#8639);
#6881=AXIS2_PLACEMENT_3D('',#16871,#8640,#8641);
#6882=AXIS2_PLACEMENT_3D('',#16872,#8642,#8643);
#6883=AXIS2_PLACEMENT_3D('',#16874,#8644,#8645);
#6884=AXIS2_PLACEMENT_3D('',#16876,#8646,#8647);
#6885=AXIS2_PLACEMENT_3D('',#16877,#8648,#8649);
#6886=AXIS2_PLACEMENT_3D('',#16879,#8650,#8651);
#6887=AXIS2_PLACEMENT_3D('',#16881,#8653,#8654);
#6888=AXIS2_PLACEMENT_3D('',#16882,#8655,#8656);
#6889=AXIS2_PLACEMENT_3D('',#16884,#8657,#8658);
#6890=AXIS2_PLACEMENT_3D('',#16886,#8660,#8661);
#6891=AXIS2_PLACEMENT_3D('',#16887,#8662,#8663);
#6892=AXIS2_PLACEMENT_3D('',#16889,#8664,#8665);
#6893=AXIS2_PLACEMENT_3D('',#16892,#8667,#8668);
#6894=AXIS2_PLACEMENT_3D('',#16893,#8669,#8670);
#6895=AXIS2_PLACEMENT_3D('',#16895,#8671,#8672);
#6896=AXIS2_PLACEMENT_3D('',#16896,#8673,#8674);
#6897=AXIS2_PLACEMENT_3D('',#16898,#8675,#8676);
#6898=AXIS2_PLACEMENT_3D('',#16901,#8678,#8679);
#6899=AXIS2_PLACEMENT_3D('',#16902,#8680,#8681);
#6900=AXIS2_PLACEMENT_3D('',#16904,#8682,#8683);
#6901=AXIS2_PLACEMENT_3D('',#16905,#8684,#8685);
#6902=AXIS2_PLACEMENT_3D('',#16906,#8686,#8687);
#6903=AXIS2_PLACEMENT_3D('',#16908,#8688,#8689);
#6904=AXIS2_PLACEMENT_3D('',#16910,#8690,#8691);
#6905=AXIS2_PLACEMENT_3D('',#16911,#8692,#8693);
#6906=AXIS2_PLACEMENT_3D('',#16914,#8695,#8696);
#6907=AXIS2_PLACEMENT_3D('',#16915,#8697,#8698);
#6908=AXIS2_PLACEMENT_3D('',#16917,#8699,#8700);
#6909=AXIS2_PLACEMENT_3D('',#16918,#8701,#8702);
#6910=AXIS2_PLACEMENT_3D('',#16921,#8704,#8705);
#6911=AXIS2_PLACEMENT_3D('',#16922,#8706,#8707);
#6912=AXIS2_PLACEMENT_3D('',#16924,#8708,#8709);
#6913=AXIS2_PLACEMENT_3D('',#16925,#8710,#8711);
#6914=AXIS2_PLACEMENT_3D('',#16928,#8713,#8714);
#6915=AXIS2_PLACEMENT_3D('',#16929,#8715,#8716);
#6916=AXIS2_PLACEMENT_3D('',#16931,#8717,#8718);
#6917=AXIS2_PLACEMENT_3D('',#16932,#8719,#8720);
#6918=AXIS2_PLACEMENT_3D('',#16934,#8722,#8723);
#6919=AXIS2_PLACEMENT_3D('',#16936,#8724,#8725);
#6920=AXIS2_PLACEMENT_3D('',#16939,#8727,#8728);
#6921=AXIS2_PLACEMENT_3D('',#16940,#8729,#8730);
#6922=AXIS2_PLACEMENT_3D('',#16942,#8731,#8732);
#6923=AXIS2_PLACEMENT_3D('',#16943,#8733,#8734);
#6924=AXIS2_PLACEMENT_3D('',#16944,#8735,#8736);
#6925=AXIS2_PLACEMENT_3D('',#16945,#8737,#8738);
#6926=AXIS2_PLACEMENT_3D('',#16946,#8739,#8740);
#6927=AXIS2_PLACEMENT_3D('',#16947,#8741,#8742);
#6928=AXIS2_PLACEMENT_3D('',#16948,#8743,#8744);
#6929=AXIS2_PLACEMENT_3D('',#16949,#8745,#8746);
#6930=AXIS2_PLACEMENT_3D('',#16950,#8747,#8748);
#6931=AXIS2_PLACEMENT_3D('',#16951,#8749,#8750);
#6932=AXIS2_PLACEMENT_3D('',#16952,#8751,#8752);
#6933=AXIS2_PLACEMENT_3D('',#16955,#8753,#8754);
#6934=AXIS2_PLACEMENT_3D('',#16959,#8756,#8757);
#6935=AXIS2_PLACEMENT_3D('',#16963,#8759,#8760);
#6936=AXIS2_PLACEMENT_3D('',#16967,#8762,#8763);
#6937=AXIS2_PLACEMENT_3D('',#16970,#8765,#8766);
#6938=AXIS2_PLACEMENT_3D('',#16972,#8767,#8768);
#6939=AXIS2_PLACEMENT_3D('',#16973,#8769,#8770);
#6940=AXIS2_PLACEMENT_3D('',#16976,#8772,#8773);
#6941=AXIS2_PLACEMENT_3D('',#16977,#8774,#8775);
#6942=AXIS2_PLACEMENT_3D('',#16980,#8776,#8777);
#6943=AXIS2_PLACEMENT_3D('',#16984,#8779,#8780);
#6944=AXIS2_PLACEMENT_3D('',#16988,#8782,#8783);
#6945=AXIS2_PLACEMENT_3D('',#16992,#8785,#8786);
#6946=AXIS2_PLACEMENT_3D('',#16995,#8788,#8789);
#6947=AXIS2_PLACEMENT_3D('',#16996,#8790,#8791);
#6948=AXIS2_PLACEMENT_3D('',#16999,#8792,#8793);
#6949=AXIS2_PLACEMENT_3D('',#17002,#8796,#8797);
#6950=AXIS2_PLACEMENT_3D('',#17005,#8798,#8799);
#6951=AXIS2_PLACEMENT_3D('',#17009,#8801,#8802);
#6952=AXIS2_PLACEMENT_3D('',#17013,#8804,#8805);
#6953=AXIS2_PLACEMENT_3D('',#17017,#8807,#8808);
#6954=AXIS2_PLACEMENT_3D('',#17022,#8811,#8812);
#6955=AXIS2_PLACEMENT_3D('',#17026,#8814,#8815);
#6956=AXIS2_PLACEMENT_3D('',#17030,#8817,#8818);
#6957=AXIS2_PLACEMENT_3D('',#17032,#8820,#8821);
#6958=AXIS2_PLACEMENT_3D('',#17035,#8824,#8825);
#6959=AXIS2_PLACEMENT_3D('',#17037,#8827,#8828);
#6960=AXIS2_PLACEMENT_3D('',#17039,#8830,#8831);
#6961=AXIS2_PLACEMENT_3D('',#17041,#8833,#8834);
#6962=AXIS2_PLACEMENT_3D('',#17043,#8836,#8837);
#6963=AXIS2_PLACEMENT_3D('',#17045,#8839,#8840);
#6964=AXIS2_PLACEMENT_3D('',#17047,#8842,#8843);
#6965=AXIS2_PLACEMENT_3D('',#17048,#8844,#8845);
#6966=AXIS2_PLACEMENT_3D('',#17050,#8847,#8848);
#6967=AXIS2_PLACEMENT_3D('',#17052,#8850,#8851);
#6968=AXIS2_PLACEMENT_3D('',#17054,#8853,#8854);
#6969=AXIS2_PLACEMENT_3D('',#17056,#8856,#8857);
#6970=AXIS2_PLACEMENT_3D('',#17058,#8859,#8860);
#6971=AXIS2_PLACEMENT_3D('',#17060,#8862,#8863);
#6972=AXIS2_PLACEMENT_3D('',#17061,#8864,#8865);
#6973=AXIS2_PLACEMENT_3D('',#17063,#8867,#8868);
#6974=AXIS2_PLACEMENT_3D('',#17064,#8869,#8870);
#6975=AXIS2_PLACEMENT_3D('',#17065,#8871,#8872);
#6976=AXIS2_PLACEMENT_3D('',#17066,#8873,#8874);
#6977=AXIS2_PLACEMENT_3D('',#17067,#8875,#8876);
#6978=DIRECTION('axis',(0.,0.,1.));
#6979=DIRECTION('refdir',(1.,0.,0.));
#6980=DIRECTION('axis',(0.,0.,1.));
#6981=DIRECTION('refdir',(1.,0.,0.));
#6982=DIRECTION('center_axis',(0.,0.,1.));
#6983=DIRECTION('ref_axis',(1.,0.,0.));
#6984=DIRECTION('',(1.,0.,0.));
#6985=DIRECTION('',(0.,1.,0.));
#6986=DIRECTION('',(1.,0.,0.));
#6987=DIRECTION('',(0.,-1.,0.));
#6988=DIRECTION('center_axis',(0.,0.707106781186548,-0.707106781186548));
#6989=DIRECTION('ref_axis',(0.,0.707106781186548,0.707106781186548));
#6990=DIRECTION('',(-0.577350269189626,-0.577350269189626,-0.577350269189626));
#6991=DIRECTION('',(1.,0.,0.));
#6992=DIRECTION('',(0.577350269189626,-0.577350269189626,-0.577350269189626));
#6993=DIRECTION('center_axis',(0.707106781186548,0.707106781186548,0.));
#6994=DIRECTION('ref_axis',(0.707106781186548,-0.707106781186548,0.));
#6995=DIRECTION('',(0.654653670707987,-0.654653670707987,0.377964473009193));
#6996=DIRECTION('',(0.,0.,-1.));
#6997=DIRECTION('',(0.,0.,-1.));
#6998=DIRECTION('center_axis',(0.,-0.500000000000017,-0.866025403784429));
#6999=DIRECTION('ref_axis',(0.,0.866025403784429,-0.500000000000017));
#7000=DIRECTION('',(1.,0.,0.));
#7001=DIRECTION('',(0.,-0.866025403784429,0.500000000000017));
#7002=DIRECTION('',(-1.,0.,0.));
#7003=DIRECTION('',(0.654653670707987,0.654653670707987,-0.377964473009193));
#7004=DIRECTION('',(0.,-0.866025403784429,0.500000000000017));
#7005=DIRECTION('center_axis',(0.,0.500000000000017,0.866025403784429));
#7006=DIRECTION('ref_axis',(1.,0.,0.));
#7007=DIRECTION('center_axis',(0.,0.500000000000017,0.866025403784429));
#7008=DIRECTION('ref_axis',(1.,0.,0.));
#7009=DIRECTION('center_axis',(0.,0.,1.));
#7010=DIRECTION('ref_axis',(1.,0.,0.));
#7011=DIRECTION('',(0.,-1.,0.));
#7012=DIRECTION('',(1.,0.,0.));
#7013=DIRECTION('',(0.,1.,0.));
#7014=DIRECTION('center_axis',(1.,0.,0.));
#7015=DIRECTION('ref_axis',(0.,1.,0.));
#7016=DIRECTION('',(0.,0.,1.));
#7017=DIRECTION('center_axis',(0.,-1.,0.));
#7018=DIRECTION('ref_axis',(1.,0.,0.));
#7019=DIRECTION('',(0.,0.,1.));
#7020=DIRECTION('center_axis',(0.,1.,0.));
#7021=DIRECTION('ref_axis',(0.,0.,-1.));
#7022=DIRECTION('center_axis',(0.,1.,0.));
#7023=DIRECTION('ref_axis',(0.,0.,-1.));
#7024=DIRECTION('center_axis',(0.,1.,0.));
#7025=DIRECTION('ref_axis',(0.,0.,-1.));
#7026=DIRECTION('center_axis',(0.,1.,0.));
#7027=DIRECTION('ref_axis',(0.,0.,-1.));
#7028=DIRECTION('center_axis',(-1.,0.,0.));
#7029=DIRECTION('ref_axis',(0.,-1.,0.));
#7030=DIRECTION('',(0.,0.,-1.));
#7031=DIRECTION('center_axis',(-0.707106781186548,0.707106781186548,0.));
#7032=DIRECTION('ref_axis',(0.707106781186548,0.707106781186548,0.));
#7033=DIRECTION('',(0.,0.,-1.));
#7034=DIRECTION('center_axis',(0.,1.,0.));
#7035=DIRECTION('ref_axis',(-1.,0.,0.));
#7036=DIRECTION('center_axis',(0.,1.,0.));
#7037=DIRECTION('ref_axis',(0.,0.,-1.));
#7038=DIRECTION('center_axis',(0.,1.,0.));
#7039=DIRECTION('ref_axis',(0.,0.,-1.));
#7040=DIRECTION('center_axis',(0.,1.,0.));
#7041=DIRECTION('ref_axis',(0.,0.,-1.));
#7042=DIRECTION('center_axis',(0.,1.,0.));
#7043=DIRECTION('ref_axis',(0.,0.,-1.));
#7044=DIRECTION('center_axis',(0.,1.,0.));
#7045=DIRECTION('ref_axis',(0.,0.,-1.));
#7046=DIRECTION('',(0.,1.,0.));
#7047=DIRECTION('center_axis',(0.,1.,0.));
#7048=DIRECTION('ref_axis',(0.,0.,-1.));
#7049=DIRECTION('',(0.,1.,0.));
#7050=DIRECTION('center_axis',(0.,1.,0.));
#7051=DIRECTION('ref_axis',(0.,0.,-1.));
#7052=DIRECTION('',(0.,1.,0.));
#7053=DIRECTION('center_axis',(0.,1.,0.));
#7054=DIRECTION('ref_axis',(0.,0.,-1.));
#7055=DIRECTION('',(0.,1.,0.));
#7056=DIRECTION('center_axis',(0.,0.500000000000017,0.866025403784429));
#7057=DIRECTION('ref_axis',(1.,0.,0.));
#7058=DIRECTION('center_axis',(0.,0.500000000000017,0.866025403784429));
#7059=DIRECTION('ref_axis',(1.,0.,0.));
#7060=DIRECTION('',(0.,0.500000000000017,0.866025403784429));
#7061=DIRECTION('center_axis',(0.,0.500000000000017,0.866025403784429));
#7062=DIRECTION('ref_axis',(1.,0.,0.));
#7063=DIRECTION('center_axis',(0.,0.500000000000017,0.866025403784429));
#7064=DIRECTION('ref_axis',(1.,0.,0.));
#7065=DIRECTION('center_axis',(0.,0.500000000000017,0.866025403784429));
#7066=DIRECTION('ref_axis',(1.,0.,0.));
#7067=DIRECTION('center_axis',(0.,0.500000000000017,0.866025403784429));
#7068=DIRECTION('ref_axis',(1.,0.,0.));
#7069=DIRECTION('',(0.,0.500000000000017,0.866025403784429));
#7070=DIRECTION('axis',(0.,0.,1.));
#7071=DIRECTION('refdir',(1.,0.,0.));
#7072=DIRECTION('axis',(0.,0.,1.));
#7073=DIRECTION('refdir',(1.,0.,0.));
#7074=DIRECTION('center_axis',(0.,1.,0.));
#7075=DIRECTION('ref_axis',(1.,0.,0.));
#7076=DIRECTION('center_axis',(0.,1.,0.));
#7077=DIRECTION('ref_axis',(0.,0.,-1.));
#7078=DIRECTION('',(-1.,0.,0.));
#7079=DIRECTION('center_axis',(0.,1.,0.));
#7080=DIRECTION('ref_axis',(1.,0.,0.));
#7081=DIRECTION('',(0.,0.,-1.));
#7082=DIRECTION('center_axis',(0.,1.,0.));
#7083=DIRECTION('ref_axis',(0.,0.,1.));
#7084=DIRECTION('',(1.,0.,0.));
#7085=DIRECTION('center_axis',(0.,1.,0.));
#7086=DIRECTION('ref_axis',(-1.,0.,0.));
#7087=DIRECTION('',(0.,0.,1.));
#7088=DIRECTION('center_axis',(0.,-1.,0.));
#7089=DIRECTION('ref_axis',(1.,0.,0.));
#7090=DIRECTION('center_axis',(0.,-1.,0.));
#7091=DIRECTION('ref_axis',(1.,0.,0.));
#7092=DIRECTION('center_axis',(0.,-1.,0.));
#7093=DIRECTION('ref_axis',(1.,0.,0.));
#7094=DIRECTION('center_axis',(0.,-1.,0.));
#7095=DIRECTION('ref_axis',(1.,0.,0.));
#7096=DIRECTION('center_axis',(0.,-1.,0.));
#7097=DIRECTION('ref_axis',(1.,0.,0.));
#7098=DIRECTION('center_axis',(0.,-1.,0.));
#7099=DIRECTION('ref_axis',(1.,0.,0.));
#7100=DIRECTION('center_axis',(0.,1.,0.));
#7101=DIRECTION('ref_axis',(1.,0.,0.));
#7102=DIRECTION('',(0.,1.,0.));
#7103=DIRECTION('center_axis',(0.,-1.,0.));
#7104=DIRECTION('ref_axis',(1.,0.,0.));
#7105=DIRECTION('center_axis',(0.,1.,0.));
#7106=DIRECTION('ref_axis',(1.,0.,0.));
#7107=DIRECTION('center_axis',(0.,1.,0.));
#7108=DIRECTION('ref_axis',(1.,0.,0.));
#7109=DIRECTION('',(-1.,-1.086597479022E-12,-1.086802443273E-12));
#7110=DIRECTION('center_axis',(0.,1.,0.));
#7111=DIRECTION('ref_axis',(0.,0.,-1.));
#7112=DIRECTION('',(-1.086583814739E-12,-1.086583814739E-12,1.));
#7113=DIRECTION('center_axis',(0.,1.,0.));
#7114=DIRECTION('ref_axis',(-1.,0.,0.));
#7115=DIRECTION('',(1.,-1.086583814739E-12,1.086802443273E-12));
#7116=DIRECTION('center_axis',(0.,1.,0.));
#7117=DIRECTION('ref_axis',(0.,0.,1.));
#7118=DIRECTION('',(1.086583814739E-12,-1.086597479022E-12,-1.));
#7119=DIRECTION('center_axis',(0.,-1.,0.));
#7120=DIRECTION('ref_axis',(1.,0.,0.));
#7121=DIRECTION('center_axis',(0.,-1.,0.));
#7122=DIRECTION('ref_axis',(1.,0.,0.));
#7123=DIRECTION('center_axis',(0.,-1.,0.));
#7124=DIRECTION('ref_axis',(1.,0.,0.));
#7125=DIRECTION('center_axis',(0.,-1.,0.));
#7126=DIRECTION('ref_axis',(1.,0.,0.));
#7127=DIRECTION('center_axis',(0.,-1.,0.));
#7128=DIRECTION('ref_axis',(1.,0.,0.));
#7129=DIRECTION('center_axis',(0.,1.,0.));
#7130=DIRECTION('ref_axis',(1.,0.,0.));
#7131=DIRECTION('',(0.,1.,0.));
#7132=DIRECTION('center_axis',(0.,1.,0.));
#7133=DIRECTION('ref_axis',(1.,0.,0.));
#7134=DIRECTION('',(0.,1.,0.));
#7135=DIRECTION('center_axis',(0.,1.,0.));
#7136=DIRECTION('ref_axis',(1.,0.,0.));
#7137=DIRECTION('',(0.,1.,0.));
#7138=DIRECTION('center_axis',(0.,1.,0.));
#7139=DIRECTION('ref_axis',(1.,0.,0.));
#7140=DIRECTION('',(0.,1.,0.));
#7141=DIRECTION('center_axis',(0.,1.,0.));
#7142=DIRECTION('ref_axis',(1.,0.,0.));
#7143=DIRECTION('',(0.,1.,0.));
#7144=DIRECTION('center_axis',(0.,-1.,0.));
#7145=DIRECTION('ref_axis',(0.,0.,-1.));
#7146=DIRECTION('',(0.707106781186548,-0.707106781186548,-2.27691040135715E-10));
#7147=DIRECTION('center_axis',(0.,1.,0.));
#7148=DIRECTION('ref_axis',(1.,0.,0.));
#7149=DIRECTION('',(2.49493972053399E-10,-0.707106781186498,-0.707106781186598));
#7150=DIRECTION('center_axis',(0.,0.707106781186548,-0.707106781186548));
#7151=DIRECTION('ref_axis',(0.,-0.707106781186548,-0.707106781186548));
#7152=DIRECTION('',(-1.,-1.018672326296E-12,-1.01880896913E-12));
#7153=DIRECTION('',(-2.27688527987815E-10,-0.707106781186548,-0.707106781186548));
#7154=DIRECTION('center_axis',(0.,-1.,0.));
#7155=DIRECTION('ref_axis',(0.,0.,-1.));
#7156=DIRECTION('center_axis',(0.,1.,0.));
#7157=DIRECTION('ref_axis',(0.,0.,-1.));
#7158=DIRECTION('',(-0.707106781186548,-0.707106781186548,-2.49493972053417E-10));
#7159=DIRECTION('center_axis',(-0.707106781186548,0.707106781186548,0.));
#7160=DIRECTION('ref_axis',(-0.707106781186548,-0.707106781186548,0.));
#7161=DIRECTION('',(-1.018590340596E-12,-1.018658662013E-12,1.));
#7162=DIRECTION('',(-0.707106781186548,-0.707106781186548,2.27691040135715E-10));
#7163=DIRECTION('center_axis',(0.,-1.,0.));
#7164=DIRECTION('ref_axis',(-0.707106781142795,0.,0.7071067812303));
#7165=DIRECTION('center_axis',(0.,1.,0.));
#7166=DIRECTION('ref_axis',(-1.,0.,0.));
#7167=DIRECTION('',(-2.49493972053399E-10,-0.707106781186498,0.707106781186598));
#7168=DIRECTION('center_axis',(0.,0.707106781186548,0.707106781186548));
#7169=DIRECTION('ref_axis',(0.,-0.707106781186548,0.707106781186548));
#7170=DIRECTION('',(1.,-1.018672326296E-12,1.01880896913E-12));
#7171=DIRECTION('',(2.27688527987815E-10,-0.707106781186548,0.707106781186548));
#7172=DIRECTION('center_axis',(0.,-1.,0.));
#7173=DIRECTION('ref_axis',(0.7071067812303,0.,0.707106781142795));
#7174=DIRECTION('center_axis',(0.,1.,0.));
#7175=DIRECTION('ref_axis',(0.,0.,1.));
#7176=DIRECTION('',(0.707106781186548,-0.707106781186548,2.49496484201317E-10));
#7177=DIRECTION('center_axis',(0.707106781186548,0.707106781186548,0.));
#7178=DIRECTION('ref_axis',(0.707106781186548,-0.707106781186548,0.));
#7179=DIRECTION('',(1.018590340596E-12,-1.018672326296E-12,-1.));
#7180=DIRECTION('center_axis',(1.,0.,0.));
#7181=DIRECTION('ref_axis',(0.,0.,-1.));
#7182=DIRECTION('',(-3.916511559356E-11,1.,-2.646281416115E-9));
#7183=DIRECTION('',(-2.261124620821E-11,1.,2.415008637458E-9));
#7184=DIRECTION('center_axis',(0.,1.,0.));
#7185=DIRECTION('ref_axis',(1.,0.,0.));
#7186=DIRECTION('',(-2.646279639758E-9,1.,3.91668919504E-11));
#7187=DIRECTION('center_axis',(0.,0.,-1.));
#7188=DIRECTION('ref_axis',(-1.,0.,0.));
#7189=DIRECTION('',(2.415006861102E-9,1.,2.261124620821E-11));
#7190=DIRECTION('center_axis',(0.,1.,0.));
#7191=DIRECTION('ref_axis',(-0.707106781219254,0.,-0.707106781153841));
#7192=DIRECTION('',(3.916511559356E-11,1.,2.646279639758E-9));
#7193=DIRECTION('center_axis',(-1.,0.,0.));
#7194=DIRECTION('ref_axis',(0.,0.,1.));
#7195=DIRECTION('',(2.261124620821E-11,1.,-2.415008637458E-9));
#7196=DIRECTION('center_axis',(0.,1.,0.));
#7197=DIRECTION('ref_axis',(-0.707106781153841,0.,0.707106781219254));
#7198=DIRECTION('',(2.646279639758E-9,1.,-3.91668919504E-11));
#7199=DIRECTION('center_axis',(0.,0.,1.));
#7200=DIRECTION('ref_axis',(1.,0.,0.));
#7201=DIRECTION('',(-2.415006861102E-9,1.,-2.261124620821E-11));
#7202=DIRECTION('center_axis',(0.,1.,0.));
#7203=DIRECTION('ref_axis',(1.,0.,0.));
#7204=DIRECTION('center_axis',(0.,1.,0.));
#7205=DIRECTION('ref_axis',(-1.,0.,0.));
#7206=DIRECTION('center_axis',(0.,1.,0.));
#7207=DIRECTION('ref_axis',(1.,0.,0.));
#7208=DIRECTION('',(0.,-1.,0.));
#7209=DIRECTION('center_axis',(0.,1.,0.));
#7210=DIRECTION('ref_axis',(1.,0.,0.));
#7211=DIRECTION('center_axis',(0.,1.,0.));
#7212=DIRECTION('ref_axis',(-1.,0.,0.));
#7213=DIRECTION('center_axis',(0.,-1.,0.));
#7214=DIRECTION('ref_axis',(1.,0.,0.));
#7215=DIRECTION('center_axis',(0.,1.,0.));
#7216=DIRECTION('ref_axis',(-1.,0.,0.));
#7217=DIRECTION('center_axis',(0.,1.,0.));
#7218=DIRECTION('ref_axis',(1.,0.,0.));
#7219=DIRECTION('',(0.,-1.,0.));
#7220=DIRECTION('center_axis',(0.,1.,0.));
#7221=DIRECTION('ref_axis',(1.,0.,0.));
#7222=DIRECTION('center_axis',(0.,1.,0.));
#7223=DIRECTION('ref_axis',(-1.,0.,0.));
#7224=DIRECTION('center_axis',(0.,-1.,0.));
#7225=DIRECTION('ref_axis',(1.,0.,0.));
#7226=DIRECTION('axis',(0.,0.,1.));
#7227=DIRECTION('refdir',(1.,0.,0.));
#7228=DIRECTION('center_axis',(0.,0.,1.));
#7229=DIRECTION('ref_axis',(1.,0.,0.));
#7230=DIRECTION('',(1.,0.,0.));
#7231=DIRECTION('',(0.,-1.,0.));
#7232=DIRECTION('',(-1.,0.,0.));
#7233=DIRECTION('',(-1.,0.,0.));
#7234=DIRECTION('',(0.,1.,0.));
#7235=DIRECTION('center_axis',(0.,0.,1.));
#7236=DIRECTION('ref_axis',(1.,0.,0.));
#7237=DIRECTION('center_axis',(0.,0.,1.));
#7238=DIRECTION('ref_axis',(1.,0.,0.));
#7239=DIRECTION('',(0.,0.,-1.));
#7240=DIRECTION('center_axis',(0.,0.,-1.));
#7241=DIRECTION('ref_axis',(-1.,0.,0.));
#7242=DIRECTION('center_axis',(0.,0.,-1.));
#7243=DIRECTION('ref_axis',(-1.,0.,0.));
#7244=DIRECTION('center_axis',(0.,0.,1.));
#7245=DIRECTION('ref_axis',(-0.998822100792863,-0.0485222729035968,0.));
#7246=DIRECTION('center_axis',(-0.0485222729035999,0.998822100792863,0.));
#7247=DIRECTION('ref_axis',(0.998822100792863,0.0485222729035999,0.));
#7248=DIRECTION('center_axis',(0.,0.,-1.));
#7249=DIRECTION('ref_axis',(-1.,0.,0.));
#7250=DIRECTION('center_axis',(0.,0.,1.));
#7251=DIRECTION('ref_axis',(1.,0.,0.));
#7252=DIRECTION('center_axis',(0.,0.,1.));
#7253=DIRECTION('ref_axis',(1.,0.,0.));
#7254=DIRECTION('center_axis',(0.,0.,1.));
#7255=DIRECTION('ref_axis',(1.,0.,0.));
#7256=DIRECTION('',(0.,0.,1.));
#7257=DIRECTION('center_axis',(0.,0.,1.));
#7258=DIRECTION('ref_axis',(1.,0.,0.));
#7259=DIRECTION('center_axis',(0.,0.,1.));
#7260=DIRECTION('ref_axis',(1.,0.,0.));
#7261=DIRECTION('center_axis',(0.,0.,1.));
#7262=DIRECTION('ref_axis',(-1.,0.,0.));
#7263=DIRECTION('center_axis',(0.,0.,1.));
#7264=DIRECTION('ref_axis',(-0.99941623957466,0.0341640172468879,0.));
#7265=DIRECTION('center_axis',(0.0341640172468871,0.99941623957466,0.));
#7266=DIRECTION('ref_axis',(0.99941623957466,-0.0341640172468871,0.));
#7267=DIRECTION('center_axis',(0.,0.,1.));
#7268=DIRECTION('ref_axis',(-1.,0.,0.));
#7269=DIRECTION('center_axis',(0.,0.,1.));
#7270=DIRECTION('ref_axis',(-1.,0.,0.));
#7271=DIRECTION('center_axis',(0.,0.,1.));
#7272=DIRECTION('ref_axis',(1.,0.,0.));
#7273=DIRECTION('',(0.,0.,-1.));
#7274=DIRECTION('center_axis',(0.,0.,1.));
#7275=DIRECTION('ref_axis',(1.,0.,0.));
#7276=DIRECTION('center_axis',(0.,0.,1.));
#7277=DIRECTION('ref_axis',(1.,0.,0.));
#7278=DIRECTION('',(0.,1.,0.));
#7279=DIRECTION('',(-1.,0.,0.));
#7280=DIRECTION('',(0.,-1.,0.));
#7281=DIRECTION('',(1.,0.,0.));
#7282=DIRECTION('',(1.,0.,0.));
#7283=DIRECTION('center_axis',(0.,1.,0.));
#7284=DIRECTION('ref_axis',(0.,0.,1.));
#7285=DIRECTION('',(0.,1.,0.));
#7286=DIRECTION('center_axis',(0.,1.,0.));
#7287=DIRECTION('ref_axis',(0.,0.,1.));
#7288=DIRECTION('center_axis',(0.,-1.,0.));
#7289=DIRECTION('ref_axis',(1.,0.,0.));
#7290=DIRECTION('center_axis',(1.,0.,0.));
#7291=DIRECTION('ref_axis',(0.,1.,0.));
#7292=DIRECTION('',(0.,0.,-1.));
#7293=DIRECTION('',(0.,-1.,0.));
#7294=DIRECTION('',(0.,0.,-1.));
#7295=DIRECTION('center_axis',(0.,0.,-1.));
#7296=DIRECTION('ref_axis',(1.,0.,0.));
#7297=DIRECTION('center_axis',(0.,0.,1.));
#7298=DIRECTION('ref_axis',(0.,-1.,0.));
#7299=DIRECTION('',(0.,0.,-1.));
#7300=DIRECTION('center_axis',(0.,0.,-1.));
#7301=DIRECTION('ref_axis',(1.,0.,0.));
#7302=DIRECTION('center_axis',(0.707106781186545,0.70710678118655,0.));
#7303=DIRECTION('ref_axis',(0.707106781186545,-0.70710678118655,0.));
#7304=DIRECTION('center_axis',(1.,0.,0.));
#7305=DIRECTION('ref_axis',(0.,-1.,0.));
#7306=DIRECTION('center_axis',(0.,-1.,0.));
#7307=DIRECTION('ref_axis',(0.,0.,-1.));
#7308=DIRECTION('center_axis',(-1.,0.,0.));
#7309=DIRECTION('ref_axis',(0.,0.,-1.));
#7310=DIRECTION('',(-1.,0.,2.676881426896E-11));
#7311=DIRECTION('center_axis',(-0.999999999999956,-2.96157146246387E-7,
0.));
#7312=DIRECTION('ref_axis',(-5.76584526410216E-19,1.94688709598283E-12,
-1.));
#7313=DIRECTION('center_axis',(-1.,0.,0.));
#7314=DIRECTION('ref_axis',(0.,0.,-1.));
#7315=DIRECTION('center_axis',(-1.,0.,0.));
#7316=DIRECTION('ref_axis',(0.,0.,-1.));
#7317=DIRECTION('',(-1.,0.,-2.67704677823E-11));
#7318=DIRECTION('center_axis',(-1.,0.,0.));
#7319=DIRECTION('ref_axis',(0.,0.,-1.));
#7320=DIRECTION('center_axis',(0.,-1.,0.));
#7321=DIRECTION('ref_axis',(1.,0.,0.));
#7322=DIRECTION('',(1.,0.,2.67704677823E-11));
#7323=DIRECTION('center_axis',(0.,-1.,0.));
#7324=DIRECTION('ref_axis',(0.261958162689304,0.,-0.965079230426416));
#7325=DIRECTION('center_axis',(0.,-1.,0.));
#7326=DIRECTION('ref_axis',(0.261958162689304,0.,-0.965079230426416));
#7327=DIRECTION('center_axis',(0.,-1.,0.));
#7328=DIRECTION('ref_axis',(1.,0.,0.));
#7329=DIRECTION('center_axis',(0.,-1.,0.));
#7330=DIRECTION('ref_axis',(-0.261958162689304,0.,0.965079230426416));
#7331=DIRECTION('',(1.,0.,-2.676881426896E-11));
#7332=DIRECTION('',(0.,0.,-1.));
#7333=DIRECTION('center_axis',(0.,1.,0.));
#7334=DIRECTION('ref_axis',(-0.999130476717975,0.,0.0416928110507389));
#7335=DIRECTION('center_axis',(0.0416928110507391,0.,0.999130476717975));
#7336=DIRECTION('ref_axis',(0.999130476717975,0.,-0.0416928110507391));
#7337=DIRECTION('center_axis',(0.,-1.,0.));
#7338=DIRECTION('ref_axis',(-1.,0.,0.));
#7339=DIRECTION('center_axis',(0.,-1.,0.));
#7340=DIRECTION('ref_axis',(-1.,0.,0.));
#7341=DIRECTION('center_axis',(0.999999999999956,-2.96157145634487E-7,0.));
#7342=DIRECTION('ref_axis',(5.76584525218915E-19,1.94688709598283E-12,1.));
#7343=DIRECTION('center_axis',(1.,0.,0.));
#7344=DIRECTION('ref_axis',(0.,0.,1.));
#7345=DIRECTION('center_axis',(1.,0.,0.));
#7346=DIRECTION('ref_axis',(0.,0.,1.));
#7347=DIRECTION('center_axis',(1.,0.,0.));
#7348=DIRECTION('ref_axis',(0.,0.,1.));
#7349=DIRECTION('center_axis',(0.707106781186548,0.,-0.707106781186548));
#7350=DIRECTION('ref_axis',(0.707106781186548,0.,0.707106781186548));
#7351=DIRECTION('center_axis',(1.,0.,0.));
#7352=DIRECTION('ref_axis',(0.,0.,1.));
#7353=DIRECTION('center_axis',(-1.,0.,0.));
#7354=DIRECTION('ref_axis',(0.,-1.,0.));
#7355=DIRECTION('center_axis',(-0.707106781186545,0.70710678118655,0.));
#7356=DIRECTION('ref_axis',(-0.707106781186545,-0.70710678118655,0.));
#7357=DIRECTION('center_axis',(0.,-1.,0.));
#7358=DIRECTION('ref_axis',(0.,0.,1.));
#7359=DIRECTION('center_axis',(0.,0.,1.));
#7360=DIRECTION('ref_axis',(-1.,0.,0.));
#7361=DIRECTION('center_axis',(0.,0.,-1.));
#7362=DIRECTION('ref_axis',(0.,-1.,0.));
#7363=DIRECTION('',(0.,0.,-1.));
#7364=DIRECTION('center_axis',(0.,0.,-1.));
#7365=DIRECTION('ref_axis',(0.,-1.,0.));
#7366=DIRECTION('center_axis',(-0.707106781186548,0.,0.707106781186548));
#7367=DIRECTION('ref_axis',(-0.707106781186548,0.,-0.707106781186548));
#7368=DIRECTION('center_axis',(0.,-1.,0.));
#7369=DIRECTION('ref_axis',(-1.,0.,0.));
#7370=DIRECTION('center_axis',(0.,1.,0.));
#7371=DIRECTION('ref_axis',(0.,0.,-1.));
#7372=DIRECTION('',(0.,1.,0.));
#7373=DIRECTION('center_axis',(0.,1.,0.));
#7374=DIRECTION('ref_axis',(0.,0.,-1.));
#7375=DIRECTION('center_axis',(-1.,0.,0.));
#7376=DIRECTION('ref_axis',(0.,-1.,0.));
#7377=DIRECTION('',(0.,-1.,0.));
#7378=DIRECTION('',(0.,0.,-1.));
#7379=DIRECTION('center_axis',(0.,0.,-1.));
#7380=DIRECTION('ref_axis',(-1.,0.,0.));
#7381=DIRECTION('center_axis',(0.,0.,1.));
#7382=DIRECTION('ref_axis',(0.,1.,0.));
#7383=DIRECTION('',(0.,0.,-1.));
#7384=DIRECTION('center_axis',(0.,0.,-1.));
#7385=DIRECTION('ref_axis',(-1.,0.,0.));
#7386=DIRECTION('center_axis',(-0.707106781186545,-0.70710678118655,0.));
#7387=DIRECTION('ref_axis',(-0.707106781186545,0.70710678118655,0.));
#7388=DIRECTION('center_axis',(-1.,0.,0.));
#7389=DIRECTION('ref_axis',(0.,1.,0.));
#7390=DIRECTION('center_axis',(1.,0.,0.));
#7391=DIRECTION('ref_axis',(0.,0.,-1.));
#7392=DIRECTION('',(1.,0.,0.));
#7393=DIRECTION('center_axis',(1.,0.,0.));
#7394=DIRECTION('ref_axis',(0.,0.,-1.));
#7395=DIRECTION('center_axis',(-0.707106781186545,0.70710678118655,0.));
#7396=DIRECTION('ref_axis',(0.707106781186545,0.70710678118655,0.));
#7397=DIRECTION('center_axis',(0.,1.,0.));
#7398=DIRECTION('ref_axis',(1.,0.,0.));
#7399=DIRECTION('center_axis',(0.,0.,-1.));
#7400=DIRECTION('ref_axis',(0.,1.,0.));
#7401=DIRECTION('center_axis',(0.,-1.,0.));
#7402=DIRECTION('ref_axis',(0.,0.,-1.));
#7403=DIRECTION('center_axis',(0.,0.,-1.));
#7404=DIRECTION('ref_axis',(0.,1.,0.));
#7405=DIRECTION('',(0.,0.,-1.));
#7406=DIRECTION('center_axis',(0.,0.,1.));
#7407=DIRECTION('ref_axis',(1.,0.,0.));
#7408=DIRECTION('center_axis',(0.,1.,0.));
#7409=DIRECTION('ref_axis',(-1.,0.,0.));
#7410=DIRECTION('',(-1.,0.,0.));
#7411=DIRECTION('center_axis',(0.,1.,0.));
#7412=DIRECTION('ref_axis',(1.,0.,0.));
#7413=DIRECTION('center_axis',(-1.,0.,0.));
#7414=DIRECTION('ref_axis',(0.,0.,1.));
#7415=DIRECTION('center_axis',(-1.,0.,0.));
#7416=DIRECTION('ref_axis',(0.,0.,1.));
#7417=DIRECTION('center_axis',(1.,0.,0.));
#7418=DIRECTION('ref_axis',(0.,1.,0.));
#7419=DIRECTION('center_axis',(0.,0.70710678118655,-0.707106781186545));
#7420=DIRECTION('ref_axis',(0.,0.70710678118655,0.707106781186545));
#7421=DIRECTION('center_axis',(-0.707106781186548,0.,-0.707106781186548));
#7422=DIRECTION('ref_axis',(-0.707106781186548,0.,0.707106781186548));
#7423=DIRECTION('center_axis',(0.,1.,0.));
#7424=DIRECTION('ref_axis',(-1.,0.,0.));
#7425=DIRECTION('center_axis',(0.,-1.,0.));
#7426=DIRECTION('ref_axis',(0.,0.,1.));
#7427=DIRECTION('center_axis',(0.,1.,0.));
#7428=DIRECTION('ref_axis',(1.,0.,0.));
#7429=DIRECTION('center_axis',(0.,1.,0.));
#7430=DIRECTION('ref_axis',(1.,0.,0.));
#7431=DIRECTION('',(0.,-1.,0.));
#7432=DIRECTION('center_axis',(0.,1.,0.));
#7433=DIRECTION('ref_axis',(1.,0.,0.));
#7434=DIRECTION('center_axis',(0.,1.,0.));
#7435=DIRECTION('ref_axis',(1.,0.,0.));
#7436=DIRECTION('center_axis',(0.,1.,0.));
#7437=DIRECTION('ref_axis',(1.,0.,0.));
#7438=DIRECTION('center_axis',(0.,1.,0.));
#7439=DIRECTION('ref_axis',(1.,0.,0.));
#7440=DIRECTION('',(-0.707106781186547,0.707106781186548,8.65956056235493E-17));
#7441=DIRECTION('center_axis',(0.,1.,0.));
#7442=DIRECTION('ref_axis',(1.,0.,0.));
#7443=DIRECTION('',(0.,1.,0.));
#7444=DIRECTION('center_axis',(0.,-1.,0.));
#7445=DIRECTION('ref_axis',(-1.,0.,0.));
#7446=DIRECTION('center_axis',(0.,1.,0.));
#7447=DIRECTION('ref_axis',(-1.,0.,0.));
#7448=DIRECTION('',(-0.0697564737441253,0.997564050259824,-8.54270422905495E-18));
#7449=DIRECTION('center_axis',(0.,1.,0.));
#7450=DIRECTION('ref_axis',(-1.,0.,0.));
#7451=DIRECTION('center_axis',(0.,-1.,0.));
#7452=DIRECTION('ref_axis',(-1.,0.,0.));
#7453=DIRECTION('center_axis',(0.,1.,0.));
#7454=DIRECTION('ref_axis',(-1.,0.,0.));
#7455=DIRECTION('center_axis',(0.,1.,0.));
#7456=DIRECTION('ref_axis',(-1.,0.,0.));
#7457=DIRECTION('',(-0.0697564737441253,0.997564050259824,-8.54270422905495E-18));
#7458=DIRECTION('center_axis',(0.,1.,0.));
#7459=DIRECTION('ref_axis',(0.,0.,1.));
#7460=DIRECTION('center_axis',(0.,1.,0.));
#7461=DIRECTION('ref_axis',(0.,0.,1.));
#7462=DIRECTION('center_axis',(0.,1.,0.));
#7463=DIRECTION('ref_axis',(0.,0.,-1.));
#7464=DIRECTION('center_axis',(1.,0.,-1.22464679914735E-16));
#7465=DIRECTION('ref_axis',(1.22464679914735E-16,0.,1.));
#7466=DIRECTION('center_axis',(0.,1.,0.));
#7467=DIRECTION('ref_axis',(-0.00148595964285994,0.,-0.999998895961361));
#7468=DIRECTION('center_axis',(-0.99999889596136,0.,0.00148595964286006));
#7469=DIRECTION('ref_axis',(0.00148595964286006,0.,0.99999889596136));
#7470=DIRECTION('center_axis',(0.,1.,0.));
#7471=DIRECTION('ref_axis',(0.7520613912797,0.,0.659093061522));
#7472=DIRECTION('center_axis',(0.,1.,0.));
#7473=DIRECTION('ref_axis',(0.906252959615387,0.,-0.422735819618294));
#7474=DIRECTION('center_axis',(0.,1.,0.));
#7475=DIRECTION('ref_axis',(-0.7520613912797,0.,-0.659093061522));
#7476=DIRECTION('center_axis',(0.,1.,0.));
#7477=DIRECTION('ref_axis',(-0.906252959678649,0.,0.422735819482676));
#7478=DIRECTION('center_axis',(0.,8.267930667502E-9,-1.));
#7479=DIRECTION('ref_axis',(-1.,1.563194018672E-13,1.29243797662339E-21));
#7480=DIRECTION('center_axis',(0.,0.,-1.));
#7481=DIRECTION('ref_axis',(-1.,0.,0.));
#7482=DIRECTION('center_axis',(-1.,0.,0.));
#7483=DIRECTION('ref_axis',(0.,-1.,0.));
#7484=DIRECTION('',(0.,3.40889233658E-10,-1.));
#7485=DIRECTION('',(-5.132671782924E-14,-2.643911472987E-9,-1.));
#7486=DIRECTION('',(0.,1.,0.));
#7487=DIRECTION('',(0.,-7.255275745268E-12,1.));
#7488=DIRECTION('center_axis',(1.,0.,0.));
#7489=DIRECTION('ref_axis',(0.,1.,0.));
#7490=DIRECTION('',(0.,-1.,0.));
#7491=DIRECTION('',(0.,0.,-1.));
#7492=DIRECTION('',(0.,1.,0.));
#7493=DIRECTION('',(0.,0.,-1.));
#7494=DIRECTION('',(0.,-1.,0.));
#7495=DIRECTION('center_axis',(1.,0.,0.));
#7496=DIRECTION('ref_axis',(0.,0.,-1.));
#7497=DIRECTION('center_axis',(1.,0.,0.));
#7498=DIRECTION('ref_axis',(0.,0.,-1.));
#7499=DIRECTION('',(1.,0.,0.));
#7500=DIRECTION('',(1.,0.,0.));
#7501=DIRECTION('center_axis',(1.,0.,0.));
#7502=DIRECTION('ref_axis',(0.,0.,-1.));
#7503=DIRECTION('center_axis',(1.,0.,0.));
#7504=DIRECTION('ref_axis',(0.,0.,-1.));
#7505=DIRECTION('center_axis',(0.,0.,1.));
#7506=DIRECTION('ref_axis',(1.,0.,0.));
#7507=DIRECTION('',(0.,0.,1.));
#7508=DIRECTION('center_axis',(0.,0.,1.));
#7509=DIRECTION('ref_axis',(1.,0.,0.));
#7510=DIRECTION('center_axis',(0.,0.,1.));
#7511=DIRECTION('ref_axis',(1.,0.,0.));
#7512=DIRECTION('center_axis',(0.,0.,1.));
#7513=DIRECTION('ref_axis',(0.,1.,0.));
#7514=DIRECTION('',(1.,0.,0.));
#7515=DIRECTION('',(0.,1.,0.));
#7516=DIRECTION('center_axis',(0.,0.,1.));
#7517=DIRECTION('ref_axis',(1.,0.,0.));
#7518=DIRECTION('',(-1.,0.,0.));
#7519=DIRECTION('',(-1.,0.,0.));
#7520=DIRECTION('center_axis',(0.,0.,-1.));
#7521=DIRECTION('ref_axis',(1.,0.,0.));
#7522=DIRECTION('center_axis',(0.,0.,1.));
#7523=DIRECTION('ref_axis',(1.,0.,0.));
#7524=DIRECTION('',(0.,1.,0.));
#7525=DIRECTION('',(1.,0.,0.));
#7526=DIRECTION('',(-1.,0.,0.));
#7527=DIRECTION('',(0.,-1.,0.));
#7528=DIRECTION('',(1.,0.,0.));
#7529=DIRECTION('',(0.,1.,0.));
#7530=DIRECTION('',(-1.,0.,0.));
#7531=DIRECTION('center_axis',(0.,0.,1.));
#7532=DIRECTION('ref_axis',(1.,0.,0.));
#7533=DIRECTION('center_axis',(0.,0.,1.));
#7534=DIRECTION('ref_axis',(1.,0.,0.));
#7535=DIRECTION('',(0.,0.,1.));
#7536=DIRECTION('center_axis',(1.,0.,0.));
#7537=DIRECTION('ref_axis',(0.,0.,-1.));
#7538=DIRECTION('center_axis',(1.,0.,0.));
#7539=DIRECTION('ref_axis',(0.,0.,-1.));
#7540=DIRECTION('',(1.,0.,0.));
#7541=DIRECTION('',(1.,0.,0.));
#7542=DIRECTION('center_axis',(1.,0.,0.));
#7543=DIRECTION('ref_axis',(0.,0.,-1.));
#7544=DIRECTION('center_axis',(1.,0.,0.));
#7545=DIRECTION('ref_axis',(0.,1.,0.));
#7546=DIRECTION('',(0.,-3.676570159428E-11,1.));
#7547=DIRECTION('',(0.,-1.,0.));
#7548=DIRECTION('',(0.,0.,-1.));
#7549=DIRECTION('',(2.105217949922E-14,7.33486663786E-9,-1.));
#7550=DIRECTION('',(0.,0.,-1.));
#7551=DIRECTION('',(0.,1.,0.));
#7552=DIRECTION('',(0.,0.,-1.));
#7553=DIRECTION('center_axis',(-1.,0.,0.));
#7554=DIRECTION('ref_axis',(0.,0.866025403784429,0.500000000000017));
#7555=DIRECTION('center_axis',(1.,0.,0.));
#7556=DIRECTION('ref_axis',(0.,0.,-1.));
#7557=DIRECTION('center_axis',(0.,0.,1.));
#7558=DIRECTION('ref_axis',(-1.,0.,0.));
#7559=DIRECTION('center_axis',(0.,0.,-1.));
#7560=DIRECTION('ref_axis',(0.,-1.,0.));
#7561=DIRECTION('',(0.,0.,1.));
#7562=DIRECTION('',(0.,0.,1.));
#7563=DIRECTION('center_axis',(0.,0.,1.));
#7564=DIRECTION('ref_axis',(-1.,0.,0.));
#7565=DIRECTION('center_axis',(0.,0.,1.));
#7566=DIRECTION('ref_axis',(-1.,0.,0.));
#7567=DIRECTION('center_axis',(0.,0.,1.));
#7568=DIRECTION('ref_axis',(-1.,0.,0.));
#7569=DIRECTION('center_axis',(0.,-1.,0.));
#7570=DIRECTION('ref_axis',(0.,0.,-1.));
#7571=DIRECTION('center_axis',(-1.,0.,0.));
#7572=DIRECTION('ref_axis',(0.,1.,0.));
#7573=DIRECTION('center_axis',(0.,0.,1.));
#7574=DIRECTION('ref_axis',(1.,0.,0.));
#7575=DIRECTION('',(0.,1.,0.));
#7576=DIRECTION('',(-1.,0.,0.));
#7577=DIRECTION('',(-1.,0.,0.));
#7578=DIRECTION('',(0.,-1.,0.));
#7579=DIRECTION('',(1.,0.,0.));
#7580=DIRECTION('',(0.,-1.,0.));
#7581=DIRECTION('',(1.,0.,0.));
#7582=DIRECTION('',(0.,1.,0.));
#7583=DIRECTION('',(1.,0.,0.));
#7584=DIRECTION('center_axis',(0.,0.,1.));
#7585=DIRECTION('ref_axis',(0.,-1.,0.));
#7586=DIRECTION('center_axis',(0.,0.,-1.));
#7587=DIRECTION('ref_axis',(1.,0.,0.));
#7588=DIRECTION('center_axis',(0.,0.,1.));
#7589=DIRECTION('ref_axis',(1.,0.,0.));
#7590=DIRECTION('',(0.,0.,1.));
#7591=DIRECTION('center_axis',(0.,1.,0.));
#7592=DIRECTION('ref_axis',(0.,0.,-1.));
#7593=DIRECTION('center_axis',(0.,-1.,0.));
#7594=DIRECTION('ref_axis',(-1.,0.,0.));
#7595=DIRECTION('center_axis',(0.,-0.707106781186546,-0.70710678118655));
#7596=DIRECTION('ref_axis',(0.,0.70710678118655,-0.707106781186545));
#7597=DIRECTION('center_axis',(0.,0.,-1.));
#7598=DIRECTION('ref_axis',(-1.,0.,0.));
#7599=DIRECTION('',(4.284382407013E-8,0.,-0.999999999999999));
#7600=DIRECTION('center_axis',(0.,1.,0.));
#7601=DIRECTION('ref_axis',(-1.,0.,0.));
#7602=DIRECTION('',(-9.69930517813E-9,-3.46741652564E-14,-1.));
#7603=DIRECTION('center_axis',(0.,1.,0.));
#7604=DIRECTION('ref_axis',(-1.,0.,0.));
#7605=DIRECTION('center_axis',(0.,1.,0.));
#7606=DIRECTION('ref_axis',(-1.,0.,0.));
#7607=DIRECTION('',(5.264483512846E-9,0.,-1.));
#7608=DIRECTION('center_axis',(0.,1.,0.));
#7609=DIRECTION('ref_axis',(-1.,0.,0.));
#7610=DIRECTION('',(-1.431997384529E-9,0.,-1.));
#7611=DIRECTION('center_axis',(0.,0.,-1.));
#7612=DIRECTION('ref_axis',(-1.,0.,0.));
#7613=DIRECTION('center_axis',(0.,0.,-1.));
#7614=DIRECTION('ref_axis',(0.,1.,0.));
#7615=DIRECTION('center_axis',(0.,8.975029504145E-9,-1.));
#7616=DIRECTION('ref_axis',(0.,1.,8.975029504145E-9));
#7617=DIRECTION('center_axis',(0.,-2.92549305339806E-6,-0.999999999995721));
#7618=DIRECTION('ref_axis',(0.189648565613596,0.981852036486382,-2.87240131221794E-6));
#7619=DIRECTION('center_axis',(0.,0.,-1.));
#7620=DIRECTION('ref_axis',(0.,1.,0.));
#7621=DIRECTION('center_axis',(0.,0.,-1.));
#7622=DIRECTION('ref_axis',(0.,1.,0.));
#7623=DIRECTION('center_axis',(0.,0.707106781186547,0.707106781186548));
#7624=DIRECTION('ref_axis',(0.,0.707106781186548,-0.707106781186547));
#7625=DIRECTION('center_axis',(0.,-1.,0.));
#7626=DIRECTION('ref_axis',(0.,0.,-1.));
#7627=DIRECTION('center_axis',(0.,0.,1.));
#7628=DIRECTION('ref_axis',(0.,-1.,0.));
#7629=DIRECTION('center_axis',(1.,0.,0.));
#7630=DIRECTION('ref_axis',(0.,0.,-1.));
#7631=DIRECTION('center_axis',(0.,0.,1.));
#7632=DIRECTION('ref_axis',(0.,-1.,0.));
#7633=DIRECTION('center_axis',(0.,0.,1.));
#7634=DIRECTION('ref_axis',(0.,-1.,0.));
#7635=DIRECTION('',(0.,0.,1.));
#7636=DIRECTION('',(0.,0.,1.));
#7637=DIRECTION('center_axis',(0.,0.,-1.));
#7638=DIRECTION('ref_axis',(1.,0.,0.));
#7639=DIRECTION('center_axis',(0.,1.,0.));
#7640=DIRECTION('ref_axis',(-1.,0.,0.));
#7641=DIRECTION('center_axis',(0.,1.,0.));
#7642=DIRECTION('ref_axis',(1.,0.,0.));
#7643=DIRECTION('',(1.,0.,0.));
#7644=DIRECTION('',(0.,0.,-1.));
#7645=DIRECTION('',(-1.,0.,0.));
#7646=DIRECTION('center_axis',(0.,1.,0.));
#7647=DIRECTION('ref_axis',(1.,0.,0.));
#7648=DIRECTION('center_axis',(0.,1.,0.));
#7649=DIRECTION('ref_axis',(1.,0.,0.));
#7650=DIRECTION('center_axis',(0.,1.,0.));
#7651=DIRECTION('ref_axis',(1.,0.,0.));
#7652=DIRECTION('',(0.,1.,0.));
#7653=DIRECTION('center_axis',(0.,-1.,0.));
#7654=DIRECTION('ref_axis',(1.,0.,0.));
#7655=DIRECTION('center_axis',(0.,-1.,0.));
#7656=DIRECTION('ref_axis',(0.,0.,1.));
#7657=DIRECTION('',(0.,0.,1.));
#7658=DIRECTION('center_axis',(0.,-1.,0.));
#7659=DIRECTION('ref_axis',(-1.,0.,0.));
#7660=DIRECTION('center_axis',(0.,-1.,0.));
#7661=DIRECTION('ref_axis',(0.,0.,-1.));
#7662=DIRECTION('',(0.,0.,1.));
#7663=DIRECTION('center_axis',(0.,-1.,0.));
#7664=DIRECTION('ref_axis',(1.,0.,0.));
#7665=DIRECTION('center_axis',(0.,1.,0.));
#7666=DIRECTION('ref_axis',(1.,0.,0.));
#7667=DIRECTION('center_axis',(0.,1.,0.));
#7668=DIRECTION('ref_axis',(1.,0.,0.));
#7669=DIRECTION('',(0.,1.,0.));
#7670=DIRECTION('center_axis',(0.,1.,0.));
#7671=DIRECTION('ref_axis',(1.,0.,0.));
#7672=DIRECTION('center_axis',(0.,1.,0.));
#7673=DIRECTION('ref_axis',(-1.,0.,0.));
#7674=DIRECTION('',(-1.,0.,0.));
#7675=DIRECTION('',(0.,0.,-1.));
#7676=DIRECTION('',(1.,0.,0.));
#7677=DIRECTION('center_axis',(1.,0.,0.));
#7678=DIRECTION('ref_axis',(0.,0.,-1.));
#7679=DIRECTION('center_axis',(1.,0.,0.));
#7680=DIRECTION('ref_axis',(0.,0.,-1.));
#7681=DIRECTION('center_axis',(-0.707106781186547,0.707106781186548,0.));
#7682=DIRECTION('ref_axis',(0.707106781186547,0.707106781186548,0.));
#7683=DIRECTION('center_axis',(0.,1.,0.));
#7684=DIRECTION('ref_axis',(1.,0.,0.));
#7685=DIRECTION('center_axis',(0.,0.,-1.));
#7686=DIRECTION('ref_axis',(0.,1.,0.));
#7687=DIRECTION('center_axis',(0.,-1.,0.));
#7688=DIRECTION('ref_axis',(0.,0.,-1.));
#7689=DIRECTION('',(0.,-1.,0.));
#7690=DIRECTION('center_axis',(1.,0.,0.));
#7691=DIRECTION('ref_axis',(0.,1.,0.));
#7692=DIRECTION('',(0.,1.,0.));
#7693=DIRECTION('',(0.,0.,-1.));
#7694=DIRECTION('center_axis',(0.,1.,0.));
#7695=DIRECTION('ref_axis',(0.,0.,1.));
#7696=DIRECTION('center_axis',(0.,1.,0.));
#7697=DIRECTION('ref_axis',(0.,0.,1.));
#7698=DIRECTION('center_axis',(0.,0.707106781186548,-0.707106781186548));
#7699=DIRECTION('ref_axis',(0.,0.707106781186548,0.707106781186548));
#7700=DIRECTION('center_axis',(1.,0.,0.));
#7701=DIRECTION('ref_axis',(0.,1.,0.));
#7702=DIRECTION('center_axis',(0.,0.,1.));
#7703=DIRECTION('ref_axis',(1.,0.,0.));
#7704=DIRECTION('center_axis',(-1.,0.,0.));
#7705=DIRECTION('ref_axis',(0.,0.,1.));
#7706=DIRECTION('center_axis',(-1.,0.,0.));
#7707=DIRECTION('ref_axis',(0.,0.,1.));
#7708=DIRECTION('center_axis',(-1.,0.,0.));
#7709=DIRECTION('ref_axis',(0.,0.707106781186548,0.707106781186548));
#7710=DIRECTION('center_axis',(0.,0.,-1.));
#7711=DIRECTION('ref_axis',(0.,1.,0.));
#7712=DIRECTION('center_axis',(0.,-1.,0.));
#7713=DIRECTION('ref_axis',(0.,0.,1.));
#7714=DIRECTION('center_axis',(0.,1.,0.));
#7715=DIRECTION('ref_axis',(-1.,0.,0.));
#7716=DIRECTION('',(0.,-1.,0.));
#7717=DIRECTION('center_axis',(-1.,0.,0.));
#7718=DIRECTION('ref_axis',(0.,-1.,0.));
#7719=DIRECTION('',(0.,0.,-1.));
#7720=DIRECTION('',(0.,1.,0.));
#7721=DIRECTION('center_axis',(0.,1.,0.));
#7722=DIRECTION('ref_axis',(0.,0.,-1.));
#7723=DIRECTION('center_axis',(0.,1.,0.));
#7724=DIRECTION('ref_axis',(0.,0.,-1.));
#7725=DIRECTION('center_axis',(-0.707106781186547,-0.707106781186548,0.));
#7726=DIRECTION('ref_axis',(-0.707106781186547,0.707106781186548,0.));
#7727=DIRECTION('center_axis',(0.,0.,-1.));
#7728=DIRECTION('ref_axis',(-1.,0.,0.));
#7729=DIRECTION('center_axis',(-1.,0.,0.));
#7730=DIRECTION('ref_axis',(0.,1.,0.));
#7731=DIRECTION('center_axis',(1.,0.,0.));
#7732=DIRECTION('ref_axis',(0.,0.,-1.));
#7733=DIRECTION('center_axis',(0.,0.,-1.));
#7734=DIRECTION('ref_axis',(-1.,0.,0.));
#7735=DIRECTION('center_axis',(0.,0.,1.));
#7736=DIRECTION('ref_axis',(0.,1.,0.));
#7737=DIRECTION('center_axis',(-0.707106781186547,0.,-0.707106781186548));
#7738=DIRECTION('ref_axis',(-0.707106781186547,0.,0.707106781186548));
#7739=DIRECTION('center_axis',(-1.,0.,0.));
#7740=DIRECTION('ref_axis',(0.,0.,1.));
#7741=DIRECTION('center_axis',(-1.,0.,0.));
#7742=DIRECTION('ref_axis',(0.,0.,1.));
#7743=DIRECTION('center_axis',(1.,0.,0.));
#7744=DIRECTION('ref_axis',(0.,1.,0.));
#7745=DIRECTION('center_axis',(-1.,0.,0.));
#7746=DIRECTION('ref_axis',(0.,0.989089789751212,-0.147313909085001));
#7747=DIRECTION('center_axis',(0.,-1.,0.));
#7748=DIRECTION('ref_axis',(0.,0.,-1.));
#7749=DIRECTION('',(1.,0.,0.));
#7750=DIRECTION('center_axis',(0.,0.,-1.));
#7751=DIRECTION('ref_axis',(0.,1.,0.));
#7752=DIRECTION('',(1.,0.,0.));
#7753=DIRECTION('center_axis',(0.,1.,0.));
#7754=DIRECTION('ref_axis',(0.,0.,1.));
#7755=DIRECTION('center_axis',(-1.,0.,0.));
#7756=DIRECTION('ref_axis',(0.,-1.,0.));
#7757=DIRECTION('center_axis',(-1.,0.,0.));
#7758=DIRECTION('ref_axis',(0.,1.,0.));
#7759=DIRECTION('',(1.,0.,0.));
#7760=DIRECTION('center_axis',(-1.,0.,0.));
#7761=DIRECTION('ref_axis',(0.,1.,0.));
#7762=DIRECTION('center_axis',(-1.,0.,0.));
#7763=DIRECTION('ref_axis',(0.,-1.,0.));
#7764=DIRECTION('center_axis',(1.,0.,0.));
#7765=DIRECTION('ref_axis',(0.,1.,0.));
#7766=DIRECTION('center_axis',(1.,0.,0.));
#7767=DIRECTION('ref_axis',(0.,1.,0.));
#7768=DIRECTION('center_axis',(1.,0.,0.));
#7769=DIRECTION('ref_axis',(0.,-1.,0.));
#7770=DIRECTION('',(-1.,0.,0.));
#7771=DIRECTION('center_axis',(1.,0.,0.));
#7772=DIRECTION('ref_axis',(0.,-1.,0.));
#7773=DIRECTION('center_axis',(1.,0.,0.));
#7774=DIRECTION('ref_axis',(0.,1.,0.));
#7775=DIRECTION('center_axis',(-1.,0.,0.));
#7776=DIRECTION('ref_axis',(0.,-1.,0.));
#7777=DIRECTION('axis',(0.,0.,1.));
#7778=DIRECTION('refdir',(1.,0.,0.));
#7779=DIRECTION('center_axis',(0.,0.,1.));
#7780=DIRECTION('ref_axis',(1.,0.,0.));
#7781=DIRECTION('',(1.,0.,0.));
#7782=DIRECTION('',(0.500000000000017,-0.866025403784429,0.));
#7783=DIRECTION('',(-0.500000000000017,-0.866025403784429,0.));
#7784=DIRECTION('',(-1.,0.,0.));
#7785=DIRECTION('',(-0.500000000000017,0.866025403784429,0.));
#7786=DIRECTION('',(0.500000000000017,0.866025403784429,0.));
#7787=DIRECTION('center_axis',(0.,0.,1.));
#7788=DIRECTION('ref_axis',(1.,0.,0.));
#7789=DIRECTION('center_axis',(0.,-1.,0.));
#7790=DIRECTION('ref_axis',(1.,0.,0.));
#7791=DIRECTION('',(0.,0.,1.));
#7792=DIRECTION('',(1.,0.,0.));
#7793=DIRECTION('',(0.,0.,1.));
#7794=DIRECTION('center_axis',(-0.866025403784429,-0.500000000000017,0.));
#7795=DIRECTION('ref_axis',(0.500000000000017,-0.866025403784429,0.));
#7796=DIRECTION('',(0.500000000000017,-0.866025403784429,0.));
#7797=DIRECTION('',(0.,0.,1.));
#7798=DIRECTION('center_axis',(-0.866025403784429,0.500000000000017,0.));
#7799=DIRECTION('ref_axis',(-0.500000000000017,-0.866025403784429,0.));
#7800=DIRECTION('',(-0.500000000000017,-0.866025403784429,0.));
#7801=DIRECTION('',(0.,0.,1.));
#7802=DIRECTION('center_axis',(0.,1.,0.));
#7803=DIRECTION('ref_axis',(-1.,0.,0.));
#7804=DIRECTION('',(-1.,0.,0.));
#7805=DIRECTION('',(0.,0.,1.));
#7806=DIRECTION('center_axis',(0.866025403784429,0.500000000000017,0.));
#7807=DIRECTION('ref_axis',(-0.500000000000017,0.866025403784429,0.));
#7808=DIRECTION('',(-0.500000000000017,0.866025403784429,0.));
#7809=DIRECTION('',(0.,0.,1.));
#7810=DIRECTION('center_axis',(0.866025403784429,-0.500000000000017,0.));
#7811=DIRECTION('ref_axis',(0.500000000000017,0.866025403784429,0.));
#7812=DIRECTION('',(0.500000000000017,0.866025403784429,0.));
#7813=DIRECTION('center_axis',(0.,0.,1.));
#7814=DIRECTION('ref_axis',(1.,0.,0.));
#7815=DIRECTION('center_axis',(0.,0.,1.));
#7816=DIRECTION('ref_axis',(1.,0.,0.));
#7817=DIRECTION('center_axis',(0.,0.,1.));
#7818=DIRECTION('ref_axis',(1.,0.,0.));
#7819=DIRECTION('',(0.,0.,-1.));
#7820=DIRECTION('center_axis',(0.,0.,1.));
#7821=DIRECTION('ref_axis',(1.,0.,0.));
#7822=DIRECTION('center_axis',(0.,0.,1.));
#7823=DIRECTION('ref_axis',(1.,0.,0.));
#7824=DIRECTION('center_axis',(0.,0.,1.));
#7825=DIRECTION('ref_axis',(1.,0.,0.));
#7826=DIRECTION('',(0.,0.,-1.));
#7827=DIRECTION('center_axis',(0.,0.,1.));
#7828=DIRECTION('ref_axis',(1.,0.,0.));
#7829=DIRECTION('center_axis',(0.,0.,1.));
#7830=DIRECTION('ref_axis',(1.,0.,0.));
#7831=DIRECTION('center_axis',(0.,0.,1.));
#7832=DIRECTION('ref_axis',(1.,0.,0.));
#7833=DIRECTION('',(0.,0.,1.));
#7834=DIRECTION('center_axis',(0.,0.,1.));
#7835=DIRECTION('ref_axis',(1.,0.,0.));
#7836=DIRECTION('center_axis',(0.,0.,1.));
#7837=DIRECTION('ref_axis',(1.,0.,0.));
#7838=DIRECTION('center_axis',(0.,0.,1.));
#7839=DIRECTION('ref_axis',(1.,0.,0.));
#7840=DIRECTION('center_axis',(0.,0.,1.));
#7841=DIRECTION('ref_axis',(-1.,0.,0.));
#7842=DIRECTION('',(0.,0.,-1.));
#7843=DIRECTION('center_axis',(0.,0.,1.));
#7844=DIRECTION('ref_axis',(-1.,0.,0.));
#7845=DIRECTION('center_axis',(0.,0.,1.));
#7846=DIRECTION('ref_axis',(1.,0.,0.));
#7847=DIRECTION('center_axis',(0.,0.,-1.));
#7848=DIRECTION('ref_axis',(-1.,0.,0.));
#7849=DIRECTION('center_axis',(0.,0.,-1.));
#7850=DIRECTION('ref_axis',(-1.,0.,0.));
#7851=DIRECTION('center_axis',(0.,0.,-1.));
#7852=DIRECTION('ref_axis',(1.,0.,0.));
#7853=DIRECTION('',(0.,0.,1.));
#7854=DIRECTION('center_axis',(0.,0.,-1.));
#7855=DIRECTION('ref_axis',(1.,0.,0.));
#7856=DIRECTION('center_axis',(0.,0.,-1.));
#7857=DIRECTION('ref_axis',(-1.,0.,0.));
#7858=DIRECTION('center_axis',(0.,0.,1.));
#7859=DIRECTION('ref_axis',(1.,0.,0.));
#7860=DIRECTION('',(0.,0.,1.));
#7861=DIRECTION('',(1.,0.,0.));
#7862=DIRECTION('',(0.,0.,1.));
#7863=DIRECTION('',(1.,0.,0.));
#7864=DIRECTION('',(1.,0.,0.));
#7865=DIRECTION('',(0.,0.,-1.));
#7866=DIRECTION('',(-1.,0.,0.));
#7867=DIRECTION('',(0.,0.,1.));
#7868=DIRECTION('axis',(0.,0.,1.));
#7869=DIRECTION('refdir',(1.,0.,0.));
#7870=DIRECTION('axis',(0.,0.,1.));
#7871=DIRECTION('refdir',(1.,0.,0.));
#7872=DIRECTION('center_axis',(0.,-1.,0.));
#7873=DIRECTION('ref_axis',(0.,0.,1.));
#7874=DIRECTION('center_axis',(0.,-1.,0.));
#7875=DIRECTION('ref_axis',(0.,0.,-1.));
#7876=DIRECTION('center_axis',(0.,1.,0.));
#7877=DIRECTION('ref_axis',(0.,0.,-1.));
#7878=DIRECTION('center_axis',(0.,-1.,0.));
#7879=DIRECTION('ref_axis',(0.,0.,1.));
#7880=DIRECTION('',(0.,1.,0.));
#7881=DIRECTION('center_axis',(0.,-1.,0.));
#7882=DIRECTION('ref_axis',(0.,0.,-1.));
#7883=DIRECTION('center_axis',(0.,-1.,0.));
#7884=DIRECTION('ref_axis',(0.,0.,1.));
#7885=DIRECTION('center_axis',(0.,-1.,0.));
#7886=DIRECTION('ref_axis',(0.,0.,-1.));
#7887=DIRECTION('center_axis',(0.,1.,0.));
#7888=DIRECTION('ref_axis',(1.,0.,0.));
#7889=DIRECTION('center_axis',(0.,1.,0.));
#7890=DIRECTION('ref_axis',(1.,0.,0.));
#7891=DIRECTION('center_axis',(0.,1.,0.));
#7892=DIRECTION('ref_axis',(1.,0.,0.));
#7893=DIRECTION('center_axis',(0.,1.,0.));
#7894=DIRECTION('ref_axis',(1.,0.,0.));
#7895=DIRECTION('center_axis',(0.,1.,0.));
#7896=DIRECTION('ref_axis',(1.,0.,0.));
#7897=DIRECTION('center_axis',(0.,1.,0.));
#7898=DIRECTION('ref_axis',(1.,0.,0.));
#7899=DIRECTION('center_axis',(0.,1.,0.));
#7900=DIRECTION('ref_axis',(1.,0.,0.));
#7901=DIRECTION('center_axis',(0.,1.,0.));
#7902=DIRECTION('ref_axis',(1.,0.,0.));
#7903=DIRECTION('center_axis',(0.,-1.,0.));
#7904=DIRECTION('ref_axis',(0.,0.,1.));
#7905=DIRECTION('',(0.,-1.,0.));
#7906=DIRECTION('center_axis',(0.,-1.,0.));
#7907=DIRECTION('ref_axis',(0.,0.,-1.));
#7908=DIRECTION('center_axis',(0.,-1.,0.));
#7909=DIRECTION('ref_axis',(0.,0.,1.));
#7910=DIRECTION('center_axis',(0.,-1.,0.));
#7911=DIRECTION('ref_axis',(0.,0.,-1.));
#7912=DIRECTION('center_axis',(0.,-1.,0.));
#7913=DIRECTION('ref_axis',(0.,0.,1.));
#7914=DIRECTION('',(0.,1.,0.));
#7915=DIRECTION('center_axis',(0.,-1.,0.));
#7916=DIRECTION('ref_axis',(0.,0.,-1.));
#7917=DIRECTION('center_axis',(0.,-1.,0.));
#7918=DIRECTION('ref_axis',(0.,0.,1.));
#7919=DIRECTION('center_axis',(0.,-1.,0.));
#7920=DIRECTION('ref_axis',(0.,0.,-1.));
#7921=DIRECTION('center_axis',(0.,-1.,0.));
#7922=DIRECTION('ref_axis',(0.,0.,1.));
#7923=DIRECTION('',(0.,-1.,0.));
#7924=DIRECTION('center_axis',(0.,-1.,0.));
#7925=DIRECTION('ref_axis',(0.,0.,-1.));
#7926=DIRECTION('center_axis',(0.,-1.,0.));
#7927=DIRECTION('ref_axis',(0.,0.,1.));
#7928=DIRECTION('center_axis',(0.,-1.,0.));
#7929=DIRECTION('ref_axis',(0.,0.,-1.));
#7930=DIRECTION('center_axis',(0.,1.,0.));
#7931=DIRECTION('ref_axis',(1.,0.,0.));
#7932=DIRECTION('center_axis',(0.,1.,0.));
#7933=DIRECTION('ref_axis',(1.,0.,0.));
#7934=DIRECTION('center_axis',(0.,1.,0.));
#7935=DIRECTION('ref_axis',(1.,0.,0.));
#7936=DIRECTION('center_axis',(0.,1.,0.));
#7937=DIRECTION('ref_axis',(1.,0.,0.));
#7938=DIRECTION('center_axis',(0.,1.,0.));
#7939=DIRECTION('ref_axis',(1.,0.,0.));
#7940=DIRECTION('center_axis',(0.,1.,0.));
#7941=DIRECTION('ref_axis',(1.,0.,0.));
#7942=DIRECTION('center_axis',(0.,1.,0.));
#7943=DIRECTION('ref_axis',(1.,0.,0.));
#7944=DIRECTION('center_axis',(0.,1.,0.));
#7945=DIRECTION('ref_axis',(1.,0.,0.));
#7946=DIRECTION('center_axis',(0.,-1.,0.));
#7947=DIRECTION('ref_axis',(0.,0.,1.));
#7948=DIRECTION('',(0.,1.,0.));
#7949=DIRECTION('center_axis',(0.,-1.,0.));
#7950=DIRECTION('ref_axis',(0.,0.,-1.));
#7951=DIRECTION('center_axis',(0.,-1.,0.));
#7952=DIRECTION('ref_axis',(0.,0.,1.));
#7953=DIRECTION('center_axis',(0.,-1.,0.));
#7954=DIRECTION('ref_axis',(0.,0.,-1.));
#7955=DIRECTION('center_axis',(0.,-1.,0.));
#7956=DIRECTION('ref_axis',(0.,0.,1.));
#7957=DIRECTION('',(0.,-1.,0.));
#7958=DIRECTION('center_axis',(1.,0.,0.));
#7959=DIRECTION('ref_axis',(0.,-1.,0.));
#7960=DIRECTION('',(1.,0.,0.));
#7961=DIRECTION('center_axis',(1.,0.,0.));
#7962=DIRECTION('ref_axis',(0.,-1.,0.));
#7963=DIRECTION('',(1.,0.,0.));
#7964=DIRECTION('center_axis',(0.,1.,0.));
#7965=DIRECTION('ref_axis',(1.,0.,0.));
#7966=DIRECTION('',(0.,1.,0.));
#7967=DIRECTION('center_axis',(0.,1.,0.));
#7968=DIRECTION('ref_axis',(1.,0.,0.));
#7969=DIRECTION('',(0.,1.,0.));
#7970=DIRECTION('center_axis',(0.,1.,0.));
#7971=DIRECTION('ref_axis',(1.,0.,0.));
#7972=DIRECTION('',(0.,1.,0.));
#7973=DIRECTION('center_axis',(0.,1.,0.));
#7974=DIRECTION('ref_axis',(1.,0.,0.));
#7975=DIRECTION('',(0.,1.,0.));
#7976=DIRECTION('center_axis',(0.,1.,0.));
#7977=DIRECTION('ref_axis',(1.,0.,0.));
#7978=DIRECTION('',(0.,1.,0.));
#7979=DIRECTION('center_axis',(0.,1.,0.));
#7980=DIRECTION('ref_axis',(1.,0.,0.));
#7981=DIRECTION('',(0.,1.,0.));
#7982=DIRECTION('center_axis',(0.,1.,0.));
#7983=DIRECTION('ref_axis',(1.,0.,0.));
#7984=DIRECTION('',(0.,1.,0.));
#7985=DIRECTION('center_axis',(0.,1.,0.));
#7986=DIRECTION('ref_axis',(1.,0.,0.));
#7987=DIRECTION('',(0.,1.,0.));
#7988=DIRECTION('axis',(0.,0.,1.));
#7989=DIRECTION('refdir',(1.,0.,0.));
#7990=DIRECTION('axis',(0.,0.,1.));
#7991=DIRECTION('refdir',(1.,0.,0.));
#7992=DIRECTION('center_axis',(0.,0.,1.));
#7993=DIRECTION('ref_axis',(1.,0.,0.));
#7994=DIRECTION('center_axis',(0.,0.,1.));
#7995=DIRECTION('ref_axis',(-1.,0.,0.));
#7996=DIRECTION('',(0.,0.,-1.));
#7997=DIRECTION('center_axis',(0.,0.,1.));
#7998=DIRECTION('ref_axis',(-0.978057882858799,-0.2083333333333,0.));
#7999=DIRECTION('',(-3.360919818376E-10,-2.396404589967E-9,1.));
#8000=DIRECTION('center_axis',(0.,0.,-1.));
#8001=DIRECTION('ref_axis',(-0.990307970554214,-0.138888888888902,0.));
#8002=DIRECTION('',(0.,0.,-1.));
#8003=DIRECTION('center_axis',(0.,0.,1.));
#8004=DIRECTION('ref_axis',(1.,0.,0.));
#8005=DIRECTION('center_axis',(0.,0.,-1.));
#8006=DIRECTION('ref_axis',(-0.990307970554214,-0.138888888888902,0.));
#8007=DIRECTION('',(-0.138888888889,-0.9903079705542,0.));
#8008=DIRECTION('center_axis',(0.,0.,-1.));
#8009=DIRECTION('ref_axis',(0.990307970554214,-0.138888888888902,0.));
#8010=DIRECTION('',(-0.138888888888902,0.990307970554214,0.));
#8011=DIRECTION('center_axis',(0.,0.,-1.));
#8012=DIRECTION('ref_axis',(1.,0.,0.));
#8013=DIRECTION('center_axis',(0.,0.,-1.));
#8014=DIRECTION('ref_axis',(1.,0.,0.));
#8015=DIRECTION('center_axis',(0.,0.,1.));
#8016=DIRECTION('ref_axis',(1.,0.,0.));
#8017=DIRECTION('',(0.,0.,1.));
#8018=DIRECTION('center_axis',(0.,0.,-1.));
#8019=DIRECTION('ref_axis',(1.,0.,0.));
#8020=DIRECTION('center_axis',(0.,0.,1.));
#8021=DIRECTION('ref_axis',(1.,0.,0.));
#8022=DIRECTION('center_axis',(0.,0.,1.));
#8023=DIRECTION('ref_axis',(-0.860711630938934,-0.50909280918752,0.));
#8024=DIRECTION('',(0.138888888888902,-0.990307970554214,0.));
#8025=DIRECTION('center_axis',(0.,0.,1.));
#8026=DIRECTION('ref_axis',(-0.990307970554214,-0.138888888888902,0.));
#8027=DIRECTION('',(0.138888888888902,0.990307970554214,0.));
#8028=DIRECTION('center_axis',(0.,0.,1.));
#8029=DIRECTION('ref_axis',(1.16333808905522E-13,-1.,0.));
#8030=DIRECTION('center_axis',(-0.990307970554214,-0.138888888888902,0.));
#8031=DIRECTION('ref_axis',(0.138888888888902,-0.990307970554214,0.));
#8032=DIRECTION('',(-0.138888888888902,0.990307970554214,0.));
#8033=DIRECTION('',(-8.499803863751E-10,6.060543553496E-9,1.));
#8034=DIRECTION('center_axis',(0.990307970554214,0.138888888888902,0.));
#8035=DIRECTION('ref_axis',(-0.138888888888902,0.990307970554214,0.));
#8036=DIRECTION('',(-1.658618955119E-10,1.182636708731E-9,1.));
#8037=DIRECTION('center_axis',(-0.138888888888902,0.990307970554214,0.));
#8038=DIRECTION('ref_axis',(0.,0.,-1.));
#8039=DIRECTION('center_axis',(-0.138888888888902,0.990307970554214,0.));
#8040=DIRECTION('ref_axis',(0.,0.,-1.));
#8041=DIRECTION('center_axis',(-0.138888888888902,0.990307970554214,0.));
#8042=DIRECTION('ref_axis',(0.,0.,-1.));
#8043=DIRECTION('center_axis',(0.,0.,1.));
#8044=DIRECTION('ref_axis',(-8.09865507989116E-11,1.,0.));
#8045=DIRECTION('center_axis',(0.,0.,-1.));
#8046=DIRECTION('ref_axis',(-0.990307970554214,-0.138888888888902,0.));
#8047=DIRECTION('center_axis',(-0.138888888888902,-0.990307970554214,0.));
#8048=DIRECTION('ref_axis',(0.,0.,-1.));
#8049=DIRECTION('center_axis',(-0.138888888888902,-0.990307970554214,0.));
#8050=DIRECTION('ref_axis',(0.,0.,-1.));
#8051=DIRECTION('',(-0.138888888888902,-0.990307970554214,0.));
#8052=DIRECTION('center_axis',(-0.138888888888902,-0.990307970554214,0.));
#8053=DIRECTION('ref_axis',(0.,0.,-1.));
#8054=DIRECTION('center_axis',(0.,0.,1.));
#8055=DIRECTION('ref_axis',(0.997042419276589,-0.0768531987823992,0.));
#8056=DIRECTION('center_axis',(0.,0.,-1.));
#8057=DIRECTION('ref_axis',(0.990307970554214,-0.138888888888902,0.));
#8058=DIRECTION('center_axis',(0.,0.,1.));
#8059=DIRECTION('ref_axis',(1.,0.,0.));
#8060=DIRECTION('',(-5.942936233218E-10,-4.237442258943E-9,1.));
#8061=DIRECTION('center_axis',(0.990307970554214,-0.138888888888902,0.));
#8062=DIRECTION('ref_axis',(0.138888888888902,0.990307970554214,0.));
#8063=DIRECTION('center_axis',(0.990307970554214,-0.138888888888902,0.));
#8064=DIRECTION('ref_axis',(0.138888888888902,0.990307970554214,0.));
#8065=DIRECTION('center_axis',(1.,0.,0.));
#8066=DIRECTION('ref_axis',(0.,0.,-1.));
#8067=DIRECTION('',(1.,0.,0.));
#8068=DIRECTION('center_axis',(1.,0.,0.));
#8069=DIRECTION('ref_axis',(0.,0.,-1.));
#8070=DIRECTION('',(1.,0.,0.));
#8071=DIRECTION('center_axis',(0.,0.,1.));
#8072=DIRECTION('ref_axis',(1.,0.,0.));
#8073=DIRECTION('center_axis',(0.,0.,1.));
#8074=DIRECTION('ref_axis',(1.,0.,0.));
#8075=DIRECTION('',(0.,0.,1.));
#8076=DIRECTION('',(0.,0.,1.));
#8077=DIRECTION('center_axis',(0.,0.,-1.));
#8078=DIRECTION('ref_axis',(-1.,0.,0.));
#8079=DIRECTION('center_axis',(0.,0.,1.));
#8080=DIRECTION('ref_axis',(1.,0.,0.));
#8081=DIRECTION('center_axis',(0.,0.,1.));
#8082=DIRECTION('ref_axis',(1.,0.,0.));
#8083=DIRECTION('center_axis',(0.,0.,1.));
#8084=DIRECTION('ref_axis',(-1.,0.,0.));
#8085=DIRECTION('',(0.,0.,-1.));
#8086=DIRECTION('center_axis',(0.,0.,1.));
#8087=DIRECTION('ref_axis',(-1.,0.,0.));
#8088=DIRECTION('center_axis',(0.,0.,1.));
#8089=DIRECTION('ref_axis',(1.,0.,0.));
#8090=DIRECTION('center_axis',(0.,0.,-1.));
#8091=DIRECTION('ref_axis',(-1.,0.,0.));
#8092=DIRECTION('axis',(0.,0.,1.));
#8093=DIRECTION('refdir',(1.,0.,0.));
#8094=DIRECTION('center_axis',(0.,-1.,0.));
#8095=DIRECTION('ref_axis',(0.,0.,1.));
#8096=DIRECTION('center_axis',(0.,1.,0.));
#8097=DIRECTION('ref_axis',(0.,0.,-1.));
#8098=DIRECTION('center_axis',(0.,-1.,0.));
#8099=DIRECTION('ref_axis',(0.,0.,1.));
#8100=DIRECTION('',(0.,1.,0.));
#8101=DIRECTION('center_axis',(0.,-1.,0.));
#8102=DIRECTION('ref_axis',(0.,0.,-1.));
#8103=DIRECTION('center_axis',(0.,-1.,0.));
#8104=DIRECTION('ref_axis',(0.,0.,1.));
#8105=DIRECTION('center_axis',(0.,1.,0.));
#8106=DIRECTION('ref_axis',(0.,0.,-1.));
#8107=DIRECTION('center_axis',(0.,-1.,0.));
#8108=DIRECTION('ref_axis',(0.,0.,1.));
#8109=DIRECTION('',(0.,1.,0.));
#8110=DIRECTION('center_axis',(0.,-1.,0.));
#8111=DIRECTION('ref_axis',(0.,0.,-1.));
#8112=DIRECTION('center_axis',(0.,-1.,0.));
#8113=DIRECTION('ref_axis',(0.,0.,1.));
#8114=DIRECTION('center_axis',(0.,1.,0.));
#8115=DIRECTION('ref_axis',(0.,0.,-1.));
#8116=DIRECTION('center_axis',(0.,-1.,0.));
#8117=DIRECTION('ref_axis',(0.,0.,1.));
#8118=DIRECTION('',(0.,1.,0.));
#8119=DIRECTION('center_axis',(0.,-1.,0.));
#8120=DIRECTION('ref_axis',(0.,0.,-1.));
#8121=DIRECTION('',(0.,-1.,0.));
#8122=DIRECTION('center_axis',(0.,-1.,0.));
#8123=DIRECTION('ref_axis',(0.989743318610793,0.,-0.142857142857099));
#8124=DIRECTION('',(0.,-1.,0.));
#8125=DIRECTION('center_axis',(0.,1.,0.));
#8126=DIRECTION('ref_axis',(-0.989743318610793,0.,0.142857142857099));
#8127=DIRECTION('',(0.,-1.,0.));
#8128=DIRECTION('center_axis',(0.,-1.,0.));
#8129=DIRECTION('ref_axis',(-0.989743318610793,0.,0.142857142857099));
#8130=DIRECTION('',(0.,-1.,0.));
#8131=DIRECTION('center_axis',(0.,-1.,0.));
#8132=DIRECTION('ref_axis',(0.,0.,-1.));
#8133=DIRECTION('center_axis',(0.,0.,1.));
#8134=DIRECTION('ref_axis',(0.,-1.,0.));
#8135=DIRECTION('',(1.,0.,0.));
#8136=DIRECTION('',(-1.,0.,0.));
#8137=DIRECTION('center_axis',(0.,-1.,0.));
#8138=DIRECTION('ref_axis',(0.,0.,-1.));
#8139=DIRECTION('',(1.,0.,0.));
#8140=DIRECTION('center_axis',(0.,0.,-1.));
#8141=DIRECTION('ref_axis',(0.,1.,0.));
#8142=DIRECTION('',(-1.,0.,0.));
#8143=DIRECTION('center_axis',(0.,-1.,0.));
#8144=DIRECTION('ref_axis',(0.,0.,1.));
#8145=DIRECTION('center_axis',(0.,-1.,0.));
#8146=DIRECTION('ref_axis',(0.,0.,1.));
#8147=DIRECTION('center_axis',(0.,-1.,0.));
#8148=DIRECTION('ref_axis',(1.,0.,0.));
#8149=DIRECTION('center_axis',(0.,-1.,0.));
#8150=DIRECTION('ref_axis',(-1.,0.,0.));
#8151=DIRECTION('',(0.,1.,0.));
#8152=DIRECTION('center_axis',(0.,-1.,0.));
#8153=DIRECTION('ref_axis',(-1.,0.,0.));
#8154=DIRECTION('center_axis',(0.,-1.,0.));
#8155=DIRECTION('ref_axis',(1.,0.,0.));
#8156=DIRECTION('center_axis',(0.,1.,0.));
#8157=DIRECTION('ref_axis',(-1.,0.,0.));
#8158=DIRECTION('axis',(0.,0.,1.));
#8159=DIRECTION('refdir',(1.,0.,0.));
#8160=DIRECTION('center_axis',(0.,1.,0.));
#8161=DIRECTION('ref_axis',(1.,0.,0.));
#8162=DIRECTION('center_axis',(0.,1.,0.));
#8163=DIRECTION('ref_axis',(1.,0.,0.));
#8164=DIRECTION('center_axis',(0.,1.,0.));
#8165=DIRECTION('ref_axis',(1.,0.,0.));
#8166=DIRECTION('center_axis',(0.,1.,0.));
#8167=DIRECTION('ref_axis',(1.,0.,0.));
#8168=DIRECTION('',(0.,-1.,0.));
#8169=DIRECTION('',(0.,-1.,0.));
#8170=DIRECTION('',(0.,-1.,0.));
#8171=DIRECTION('center_axis',(1.,0.,0.));
#8172=DIRECTION('ref_axis',(0.,-1.,0.));
#8173=DIRECTION('center_axis',(1.,0.,0.));
#8174=DIRECTION('ref_axis',(0.,-1.,0.));
#8175=DIRECTION('',(-1.,0.,0.));
#8176=DIRECTION('center_axis',(1.,0.,0.));
#8177=DIRECTION('ref_axis',(0.,-1.,0.));
#8178=DIRECTION('',(-1.,0.,0.));
#8179=DIRECTION('center_axis',(1.,0.,0.));
#8180=DIRECTION('ref_axis',(0.,-1.,0.));
#8181=DIRECTION('center_axis',(0.,1.,0.));
#8182=DIRECTION('ref_axis',(1.,0.,0.));
#8183=DIRECTION('center_axis',(1.,0.,0.));
#8184=DIRECTION('ref_axis',(0.,-1.,0.));
#8185=DIRECTION('',(-1.,0.,0.));
#8186=DIRECTION('center_axis',(1.,0.,0.));
#8187=DIRECTION('ref_axis',(0.,1.,0.));
#8188=DIRECTION('center_axis',(1.,0.,0.));
#8189=DIRECTION('ref_axis',(0.,-1.,0.));
#8190=DIRECTION('center_axis',(1.,0.,0.));
#8191=DIRECTION('ref_axis',(0.,1.,0.));
#8192=DIRECTION('',(-1.,0.,0.));
#8193=DIRECTION('center_axis',(1.,0.,0.));
#8194=DIRECTION('ref_axis',(0.,-1.,0.));
#8195=DIRECTION('center_axis',(1.,0.,0.));
#8196=DIRECTION('ref_axis',(0.,-1.,0.));
#8197=DIRECTION('center_axis',(1.,0.,0.));
#8198=DIRECTION('ref_axis',(0.,-1.,0.));
#8199=DIRECTION('center_axis',(1.,0.,0.));
#8200=DIRECTION('ref_axis',(0.,-1.,0.));
#8201=DIRECTION('',(0.,0.,1.));
#8202=DIRECTION('',(1.,0.,0.));
#8203=DIRECTION('',(0.,1.,0.));
#8204=DIRECTION('',(1.,0.,0.));
#8205=DIRECTION('',(0.,-1.,0.));
#8206=DIRECTION('',(-1.,0.,0.));
#8207=DIRECTION('',(0.,0.,1.));
#8208=DIRECTION('',(1.,0.,0.));
#8209=DIRECTION('',(0.,-1.,0.));
#8210=DIRECTION('',(-1.,0.,0.));
#8211=DIRECTION('axis',(0.,0.,1.));
#8212=DIRECTION('refdir',(1.,0.,0.));
#8213=DIRECTION('axis',(0.,0.,1.));
#8214=DIRECTION('refdir',(1.,0.,0.));
#8215=DIRECTION('center_axis',(0.,0.,-1.));
#8216=DIRECTION('ref_axis',(0.,-1.,0.));
#8217=DIRECTION('',(1.,0.,0.));
#8218=DIRECTION('',(0.,-1.,0.));
#8219=DIRECTION('',(-1.,0.,0.));
#8220=DIRECTION('center_axis',(0.,0.,1.));
#8221=DIRECTION('ref_axis',(0.,1.,0.));
#8222=DIRECTION('center_axis',(1.,0.,0.));
#8223=DIRECTION('ref_axis',(0.,0.,1.));
#8224=DIRECTION('center_axis',(1.,0.,0.));
#8225=DIRECTION('ref_axis',(0.,0.,1.));
#8226=DIRECTION('center_axis',(1.,0.,0.));
#8227=DIRECTION('ref_axis',(0.,0.,1.));
#8228=DIRECTION('',(1.,0.,0.));
#8229=DIRECTION('center_axis',(1.,0.,0.));
#8230=DIRECTION('ref_axis',(0.,-1.,0.));
#8231=DIRECTION('',(0.,0.,-1.));
#8232=DIRECTION('',(0.,1.,0.));
#8233=DIRECTION('',(0.,0.,1.));
#8234=DIRECTION('center_axis',(1.,0.,0.));
#8235=DIRECTION('ref_axis',(0.,1.,0.));
#8236=DIRECTION('center_axis',(1.,0.,0.));
#8237=DIRECTION('ref_axis',(0.,0.,-1.));
#8238=DIRECTION('center_axis',(1.,0.,0.));
#8239=DIRECTION('ref_axis',(0.,-1.,0.));
#8240=DIRECTION('center_axis',(1.,0.,0.));
#8241=DIRECTION('ref_axis',(0.,-1.,0.));
#8242=DIRECTION('',(1.,0.,0.));
#8243=DIRECTION('center_axis',(0.,0.,-1.));
#8244=DIRECTION('ref_axis',(0.,-1.,0.));
#8245=DIRECTION('center_axis',(0.,0.,-1.));
#8246=DIRECTION('ref_axis',(0.,1.,0.));
#8247=DIRECTION('',(0.,0.,-1.));
#8248=DIRECTION('center_axis',(0.,0.,-1.));
#8249=DIRECTION('ref_axis',(0.,1.,0.));
#8250=DIRECTION('center_axis',(0.,0.,-1.));
#8251=DIRECTION('ref_axis',(0.,-1.,0.));
#8252=DIRECTION('center_axis',(0.,0.,1.));
#8253=DIRECTION('ref_axis',(0.,-1.,0.));
#8254=DIRECTION('center_axis',(0.,0.,-1.));
#8255=DIRECTION('ref_axis',(1.,0.,0.));
#8256=DIRECTION('center_axis',(0.,0.,-1.));
#8257=DIRECTION('ref_axis',(1.,0.,0.));
#8258=DIRECTION('center_axis',(0.,0.,-1.));
#8259=DIRECTION('ref_axis',(1.,0.,0.));
#8260=DIRECTION('center_axis',(0.,0.,-1.));
#8261=DIRECTION('ref_axis',(0.,-1.,0.));
#8262=DIRECTION('',(0.,0.,1.));
#8263=DIRECTION('center_axis',(0.,0.,-1.));
#8264=DIRECTION('ref_axis',(0.,1.,0.));
#8265=DIRECTION('center_axis',(0.,0.,-1.));
#8266=DIRECTION('ref_axis',(0.,1.,0.));
#8267=DIRECTION('center_axis',(0.,0.,-1.));
#8268=DIRECTION('ref_axis',(-0.0100738296067504,0.999949257691136,0.));
#8269=DIRECTION('center_axis',(-0.999949257691136,-0.0100738296067502,0.));
#8270=DIRECTION('ref_axis',(0.0100738296067502,-0.999949257691136,0.));
#8271=DIRECTION('center_axis',(0.,0.,-1.));
#8272=DIRECTION('ref_axis',(0.,1.,0.));
#8273=DIRECTION('center_axis',(0.,0.,-1.));
#8274=DIRECTION('ref_axis',(0.,-1.,0.));
#8275=DIRECTION('center_axis',(0.,0.,-1.));
#8276=DIRECTION('ref_axis',(1.,0.,0.));
#8277=DIRECTION('center_axis',(0.,0.,-1.));
#8278=DIRECTION('ref_axis',(1.,0.,0.));
#8279=DIRECTION('center_axis',(0.,0.,1.));
#8280=DIRECTION('ref_axis',(0.,1.,0.));
#8281=DIRECTION('center_axis',(0.,0.,-1.));
#8282=DIRECTION('ref_axis',(1.,0.,0.));
#8283=DIRECTION('center_axis',(0.,0.,-1.));
#8284=DIRECTION('ref_axis',(1.,0.,0.));
#8285=DIRECTION('',(0.,0.,-1.));
#8286=DIRECTION('center_axis',(0.,0.,-1.));
#8287=DIRECTION('ref_axis',(1.,0.,0.));
#8288=DIRECTION('',(0.,0.,-1.));
#8289=DIRECTION('center_axis',(0.,0.,-1.));
#8290=DIRECTION('ref_axis',(1.,0.,0.));
#8291=DIRECTION('',(0.,0.,-1.));
#8292=DIRECTION('center_axis',(0.,0.,-1.));
#8293=DIRECTION('ref_axis',(0.0208019280434405,0.999783616483925,0.));
#8294=DIRECTION('center_axis',(0.999783616483925,-0.0208019280434406,0.));
#8295=DIRECTION('ref_axis',(-0.0208019280434406,-0.999783616483925,0.));
#8296=DIRECTION('center_axis',(0.,0.,1.));
#8297=DIRECTION('ref_axis',(0.,1.,0.));
#8298=DIRECTION('center_axis',(0.,0.,1.));
#8299=DIRECTION('ref_axis',(0.,1.,0.));
#8300=DIRECTION('center_axis',(0.,0.,-1.));
#8301=DIRECTION('ref_axis',(0.,-1.,0.));
#8302=DIRECTION('',(0.,0.,1.));
#8303=DIRECTION('center_axis',(0.,0.,-1.));
#8304=DIRECTION('ref_axis',(0.,1.,0.));
#8305=DIRECTION('',(7.876565977693E-12,-1.341720385588E-11,1.));
#8306=DIRECTION('center_axis',(0.,0.,1.));
#8307=DIRECTION('ref_axis',(0.,1.,0.));
#8308=DIRECTION('',(-2.869570000055E-11,-1.341720385588E-11,-1.));
#8309=DIRECTION('center_axis',(1.,0.,0.));
#8310=DIRECTION('ref_axis',(0.,-1.,0.));
#8311=DIRECTION('',(1.,0.,0.));
#8312=DIRECTION('center_axis',(0.,0.,-1.));
#8313=DIRECTION('ref_axis',(0.999999999999998,-7.01586580949265E-8,0.));
#8314=DIRECTION('center_axis',(0.,0.,1.));
#8315=DIRECTION('ref_axis',(0.298065387468285,-0.954545454545451,0.));
#8316=DIRECTION('center_axis',(0.,0.,-1.));
#8317=DIRECTION('ref_axis',(0.,1.,0.));
#8318=DIRECTION('',(-1.,-3.471931990194E-12,0.));
#8319=DIRECTION('',(-1.,0.,0.));
#8320=DIRECTION('center_axis',(0.,-1.,0.));
#8321=DIRECTION('ref_axis',(0.,0.,-1.));
#8322=DIRECTION('center_axis',(0.,0.,-1.));
#8323=DIRECTION('ref_axis',(-1.,-1.05025155239247E-11,0.));
#8324=DIRECTION('center_axis',(-1.,0.,0.));
#8325=DIRECTION('ref_axis',(0.,0.,1.));
#8326=DIRECTION('center_axis',(-1.,0.,0.));
#8327=DIRECTION('ref_axis',(0.,0.,1.));
#8328=DIRECTION('',(-1.,0.,0.));
#8329=DIRECTION('center_axis',(0.,1.,0.));
#8330=DIRECTION('ref_axis',(0.,0.,1.));
#8331=DIRECTION('center_axis',(0.,0.,-1.));
#8332=DIRECTION('ref_axis',(0.,-1.,0.));
#8333=DIRECTION('center_axis',(1.,0.,0.));
#8334=DIRECTION('ref_axis',(0.,0.,1.));
#8335=DIRECTION('center_axis',(1.,0.,0.));
#8336=DIRECTION('ref_axis',(0.,0.,-1.));
#8337=DIRECTION('',(-1.,0.,0.));
#8338=DIRECTION('center_axis',(1.,0.,0.));
#8339=DIRECTION('ref_axis',(0.,0.,1.));
#8340=DIRECTION('center_axis',(0.,0.,-1.));
#8341=DIRECTION('ref_axis',(-1.,0.,0.));
#8342=DIRECTION('center_axis',(0.,0.,-1.));
#8343=DIRECTION('ref_axis',(1.,0.,0.));
#8344=DIRECTION('',(0.,0.,1.));
#8345=DIRECTION('center_axis',(0.,0.,-1.));
#8346=DIRECTION('ref_axis',(1.,0.,0.));
#8347=DIRECTION('center_axis',(0.,0.,-1.));
#8348=DIRECTION('ref_axis',(-1.,0.,0.));
#8349=DIRECTION('center_axis',(0.,0.,1.));
#8350=DIRECTION('ref_axis',(1.,0.,0.));
#8351=DIRECTION('center_axis',(0.,0.,-1.));
#8352=DIRECTION('ref_axis',(-1.,0.,0.));
#8353=DIRECTION('center_axis',(0.,0.,-1.));
#8354=DIRECTION('ref_axis',(1.,0.,0.));
#8355=DIRECTION('',(0.,0.,1.));
#8356=DIRECTION('center_axis',(0.,0.,-1.));
#8357=DIRECTION('ref_axis',(1.,0.,0.));
#8358=DIRECTION('center_axis',(0.,0.,-1.));
#8359=DIRECTION('ref_axis',(-1.,0.,0.));
#8360=DIRECTION('center_axis',(0.,0.,1.));
#8361=DIRECTION('ref_axis',(1.,0.,0.));
#8362=DIRECTION('center_axis',(0.,0.,-1.));
#8363=DIRECTION('ref_axis',(-1.,0.,0.));
#8364=DIRECTION('center_axis',(0.,0.,-1.));
#8365=DIRECTION('ref_axis',(1.,0.,0.));
#8366=DIRECTION('',(0.,0.,1.));
#8367=DIRECTION('center_axis',(0.,0.,-1.));
#8368=DIRECTION('ref_axis',(1.,0.,0.));
#8369=DIRECTION('center_axis',(0.,0.,-1.));
#8370=DIRECTION('ref_axis',(-1.,0.,0.));
#8371=DIRECTION('center_axis',(0.,0.,1.));
#8372=DIRECTION('ref_axis',(1.,0.,0.));
#8373=DIRECTION('center_axis',(1.,0.,0.));
#8374=DIRECTION('ref_axis',(0.,1.,0.));
#8375=DIRECTION('center_axis',(1.,0.,0.));
#8376=DIRECTION('ref_axis',(0.,-1.,0.));
#8377=DIRECTION('',(-1.,0.,0.));
#8378=DIRECTION('center_axis',(1.,0.,0.));
#8379=DIRECTION('ref_axis',(0.,-1.,0.));
#8380=DIRECTION('center_axis',(1.,0.,0.));
#8381=DIRECTION('ref_axis',(0.,1.,0.));
#8382=DIRECTION('center_axis',(-1.,0.,0.));
#8383=DIRECTION('ref_axis',(0.,-1.,0.));
#8384=DIRECTION('center_axis',(1.,0.,0.));
#8385=DIRECTION('ref_axis',(0.,1.,0.));
#8386=DIRECTION('center_axis',(1.,0.,0.));
#8387=DIRECTION('ref_axis',(0.,-1.,0.));
#8388=DIRECTION('',(-1.,0.,0.));
#8389=DIRECTION('center_axis',(1.,0.,0.));
#8390=DIRECTION('ref_axis',(0.,-1.,0.));
#8391=DIRECTION('center_axis',(1.,0.,0.));
#8392=DIRECTION('ref_axis',(0.,1.,0.));
#8393=DIRECTION('center_axis',(-1.,0.,0.));
#8394=DIRECTION('ref_axis',(0.,-1.,0.));
#8395=DIRECTION('axis',(0.,0.,1.));
#8396=DIRECTION('refdir',(1.,0.,0.));
#8397=DIRECTION('center_axis',(0.,1.,0.));
#8398=DIRECTION('ref_axis',(1.,0.,0.));
#8399=DIRECTION('center_axis',(0.,-1.,0.));
#8400=DIRECTION('ref_axis',(1.,0.,0.));
#8401=DIRECTION('center_axis',(0.,1.,0.));
#8402=DIRECTION('ref_axis',(1.,0.,0.));
#8403=DIRECTION('center_axis',(0.,1.,0.));
#8404=DIRECTION('ref_axis',(1.,0.,0.));
#8405=DIRECTION('center_axis',(0.,1.,0.));
#8406=DIRECTION('ref_axis',(1.,0.,0.));
#8407=DIRECTION('center_axis',(0.,1.,0.));
#8408=DIRECTION('ref_axis',(1.,0.,0.));
#8409=DIRECTION('center_axis',(0.,1.,0.));
#8410=DIRECTION('ref_axis',(1.,0.,0.));
#8411=DIRECTION('',(0.,-1.,0.));
#8412=DIRECTION('center_axis',(0.,1.,0.));
#8413=DIRECTION('ref_axis',(1.,0.,0.));
#8414=DIRECTION('center_axis',(0.,1.,0.));
#8415=DIRECTION('ref_axis',(1.,0.,0.));
#8416=DIRECTION('center_axis',(0.,1.,0.));
#8417=DIRECTION('ref_axis',(1.,0.,0.));
#8418=DIRECTION('center_axis',(0.,1.,0.));
#8419=DIRECTION('ref_axis',(1.,0.,0.));
#8420=DIRECTION('',(0.,1.,0.));
#8421=DIRECTION('center_axis',(0.,1.,0.));
#8422=DIRECTION('ref_axis',(1.,0.,0.));
#8423=DIRECTION('center_axis',(0.,1.,0.));
#8424=DIRECTION('ref_axis',(1.,0.,0.));
#8425=DIRECTION('center_axis',(0.,1.,0.));
#8426=DIRECTION('ref_axis',(1.,0.,0.));
#8427=DIRECTION('center_axis',(0.,1.,0.));
#8428=DIRECTION('ref_axis',(0.999758738295459,0.,0.0219650905273091));
#8429=DIRECTION('center_axis',(-0.021965090527309,0.,0.999758738295459));
#8430=DIRECTION('ref_axis',(-0.999758738295459,0.,-0.021965090527309));
#8431=DIRECTION('center_axis',(0.,1.,0.));
#8432=DIRECTION('ref_axis',(1.,0.,0.));
#8433=DIRECTION('center_axis',(0.,1.,0.));
#8434=DIRECTION('ref_axis',(1.,0.,0.));
#8435=DIRECTION('center_axis',(0.,1.,0.));
#8436=DIRECTION('ref_axis',(1.,0.,0.));
#8437=DIRECTION('',(0.,-1.,0.));
#8438=DIRECTION('center_axis',(0.,-1.,0.));
#8439=DIRECTION('ref_axis',(1.,0.,0.));
#8440=DIRECTION('center_axis',(0.,1.,0.));
#8441=DIRECTION('ref_axis',(1.,0.,0.));
#8442=DIRECTION('center_axis',(0.,1.,0.));
#8443=DIRECTION('ref_axis',(1.,0.,0.));
#8444=DIRECTION('center_axis',(0.,1.,0.));
#8445=DIRECTION('ref_axis',(1.,0.,0.));
#8446=DIRECTION('center_axis',(0.,1.,0.));
#8447=DIRECTION('ref_axis',(1.,0.,0.));
#8448=DIRECTION('center_axis',(0.,1.,0.));
#8449=DIRECTION('ref_axis',(1.,0.,0.));
#8450=DIRECTION('center_axis',(0.,1.,0.));
#8451=DIRECTION('ref_axis',(1.,0.,0.));
#8452=DIRECTION('',(0.,1.,0.));
#8453=DIRECTION('center_axis',(0.,1.,0.));
#8454=DIRECTION('ref_axis',(1.,0.,0.));
#8455=DIRECTION('',(0.,1.,0.));
#8456=DIRECTION('center_axis',(0.,1.,0.));
#8457=DIRECTION('ref_axis',(1.,0.,0.));
#8458=DIRECTION('',(0.,1.,0.));
#8459=DIRECTION('center_axis',(0.,1.,0.));
#8460=DIRECTION('ref_axis',(0.999953819500319,0.,0.00961035206031418));
#8461=DIRECTION('center_axis',(-0.00961035206031406,0.,0.999953819500319));
#8462=DIRECTION('ref_axis',(-0.999953819500319,0.,-0.00961035206031406));
#8463=DIRECTION('center_axis',(0.,1.,0.));
#8464=DIRECTION('ref_axis',(1.,0.,0.));
#8465=DIRECTION('center_axis',(0.,1.,0.));
#8466=DIRECTION('ref_axis',(1.,0.,0.));
#8467=DIRECTION('center_axis',(0.,1.,0.));
#8468=DIRECTION('ref_axis',(1.,0.,0.));
#8469=DIRECTION('',(0.,-1.,0.));
#8470=DIRECTION('axis',(0.,0.,1.));
#8471=DIRECTION('refdir',(1.,0.,0.));
#8472=DIRECTION('center_axis',(0.,0.,1.));
#8473=DIRECTION('ref_axis',(-1.,0.,0.));
#8474=DIRECTION('center_axis',(0.500000000000017,0.,-0.866025403784429));
#8475=DIRECTION('ref_axis',(0.866025403784429,0.,0.500000000000017));
#8476=DIRECTION('axis',(0.,0.,1.));
#8477=DIRECTION('refdir',(1.,0.,0.));
#8478=DIRECTION('center_axis',(0.,0.,1.));
#8479=DIRECTION('ref_axis',(1.,0.,0.));
#8480=DIRECTION('',(1.,0.,0.));
#8481=DIRECTION('',(0.500000000000017,-0.866025403784429,0.));
#8482=DIRECTION('',(-0.500000000000017,-0.866025403784429,0.));
#8483=DIRECTION('',(-1.,0.,0.));
#8484=DIRECTION('',(-0.500000000000017,0.866025403784429,0.));
#8485=DIRECTION('',(0.500000000000017,0.866025403784429,0.));
#8486=DIRECTION('center_axis',(0.,0.,-1.));
#8487=DIRECTION('ref_axis',(1.,0.,0.));
#8488=DIRECTION('center_axis',(0.,0.,1.));
#8489=DIRECTION('ref_axis',(1.,0.,0.));
#8490=DIRECTION('',(0.,0.,1.));
#8491=DIRECTION('center_axis',(0.,0.,-1.));
#8492=DIRECTION('ref_axis',(1.,0.,0.));
#8493=DIRECTION('center_axis',(0.,0.,1.));
#8494=DIRECTION('ref_axis',(1.,0.,0.));
#8495=DIRECTION('',(1.,0.,0.));
#8496=DIRECTION('',(0.500000000000017,0.866025403784429,0.));
#8497=DIRECTION('',(-0.500000000000017,0.866025403784429,0.));
#8498=DIRECTION('',(-1.,0.,0.));
#8499=DIRECTION('',(-0.500000000000017,-0.866025403784429,0.));
#8500=DIRECTION('',(0.500000000000017,-0.866025403784429,0.));
#8501=DIRECTION('center_axis',(0.,-1.,0.));
#8502=DIRECTION('ref_axis',(1.,0.,0.));
#8503=DIRECTION('',(0.,0.,1.));
#8504=DIRECTION('',(0.,0.,1.));
#8505=DIRECTION('center_axis',(-0.866025403784429,-0.500000000000017,0.));
#8506=DIRECTION('ref_axis',(0.500000000000017,-0.866025403784429,0.));
#8507=DIRECTION('',(0.,0.,1.));
#8508=DIRECTION('center_axis',(-0.866025403784429,0.500000000000017,0.));
#8509=DIRECTION('ref_axis',(-0.500000000000017,-0.866025403784429,0.));
#8510=DIRECTION('',(0.,0.,1.));
#8511=DIRECTION('center_axis',(0.,1.,0.));
#8512=DIRECTION('ref_axis',(-1.,0.,0.));
#8513=DIRECTION('',(0.,0.,1.));
#8514=DIRECTION('center_axis',(0.866025403784429,0.500000000000017,0.));
#8515=DIRECTION('ref_axis',(-0.500000000000017,0.866025403784429,0.));
#8516=DIRECTION('',(0.,0.,1.));
#8517=DIRECTION('center_axis',(0.866025403784429,-0.500000000000017,0.));
#8518=DIRECTION('ref_axis',(0.500000000000017,0.866025403784429,0.));
#8519=DIRECTION('center_axis',(0.,0.,1.));
#8520=DIRECTION('ref_axis',(1.,0.,0.));
#8521=DIRECTION('center_axis',(0.,0.,1.));
#8522=DIRECTION('ref_axis',(-1.,0.,0.));
#8523=DIRECTION('',(0.,0.,-1.));
#8524=DIRECTION('center_axis',(0.,0.,1.));
#8525=DIRECTION('ref_axis',(-1.,0.,0.));
#8526=DIRECTION('center_axis',(0.,0.,1.));
#8527=DIRECTION('ref_axis',(1.,0.,0.));
#8528=DIRECTION('center_axis',(0.,0.,-1.));
#8529=DIRECTION('ref_axis',(-1.,0.,0.));
#8530=DIRECTION('axis',(0.,0.,1.));
#8531=DIRECTION('refdir',(1.,0.,0.));
#8532=DIRECTION('axis',(0.,0.,1.));
#8533=DIRECTION('refdir',(1.,0.,0.));
#8534=DIRECTION('center_axis',(0.,1.,0.));
#8535=DIRECTION('ref_axis',(1.,0.,0.));
#8536=DIRECTION('center_axis',(0.,1.,0.));
#8537=DIRECTION('ref_axis',(0.,0.,1.));
#8538=DIRECTION('center_axis',(0.,1.,0.));
#8539=DIRECTION('ref_axis',(0.903507902905271,0.,0.428571428571386));
#8540=DIRECTION('center_axis',(0.,1.,0.));
#8541=DIRECTION('ref_axis',(0.903507902905271,0.,-0.428571428571386));
#8542=DIRECTION('',(-1.,0.,0.));
#8543=DIRECTION('center_axis',(0.,1.,0.));
#8544=DIRECTION('ref_axis',(0.,0.,-1.));
#8545=DIRECTION('center_axis',(0.,1.,0.));
#8546=DIRECTION('ref_axis',(-0.903507902905271,0.,-0.428571428571386));
#8547=DIRECTION('center_axis',(0.,1.,0.));
#8548=DIRECTION('ref_axis',(-0.903507902905271,0.,0.428571428571386));
#8549=DIRECTION('',(1.,0.,0.));
#8550=DIRECTION('center_axis',(0.,-1.,0.));
#8551=DIRECTION('ref_axis',(0.903507902905271,0.,0.428571428571386));
#8552=DIRECTION('center_axis',(0.,-1.,0.));
#8553=DIRECTION('ref_axis',(0.903507902905271,0.,0.428571428571386));
#8554=DIRECTION('',(0.,-1.,0.));
#8555=DIRECTION('',(0.,-1.,0.));
#8556=DIRECTION('center_axis',(0.,1.,0.));
#8557=DIRECTION('ref_axis',(1.,0.,0.));
#8558=DIRECTION('center_axis',(0.,-1.,0.));
#8559=DIRECTION('ref_axis',(0.,0.,1.));
#8560=DIRECTION('center_axis',(0.,1.,0.));
#8561=DIRECTION('ref_axis',(1.,0.,0.));
#8562=DIRECTION('',(1.,0.,0.));
#8563=DIRECTION('center_axis',(0.,-1.,0.));
#8564=DIRECTION('ref_axis',(0.628539361054693,0.,-0.777777777777791));
#8565=DIRECTION('',(-1.,0.,0.));
#8566=DIRECTION('center_axis',(0.,-1.,0.));
#8567=DIRECTION('ref_axis',(0.,0.,-1.));
#8568=DIRECTION('center_axis',(0.,1.,0.));
#8569=DIRECTION('ref_axis',(0.903507902905271,0.,0.428571428571386));
#8570=DIRECTION('center_axis',(0.,1.,0.));
#8571=DIRECTION('ref_axis',(1.,0.,0.));
#8572=DIRECTION('center_axis',(0.,-1.,0.));
#8573=DIRECTION('ref_axis',(-0.903507902905271,0.,-0.428571428571386));
#8574=DIRECTION('',(-1.,0.,0.));
#8575=DIRECTION('center_axis',(0.,-1.,0.));
#8576=DIRECTION('ref_axis',(-0.628539361054693,0.,0.777777777777791));
#8577=DIRECTION('',(1.,0.,0.));
#8578=DIRECTION('center_axis',(0.,-1.,0.));
#8579=DIRECTION('ref_axis',(0.,0.,1.));
#8580=DIRECTION('center_axis',(0.,1.,0.));
#8581=DIRECTION('ref_axis',(-0.903507902905271,0.,-0.428571428571386));
#8582=DIRECTION('center_axis',(0.,-1.,0.));
#8583=DIRECTION('ref_axis',(0.,0.,-1.));
#8584=DIRECTION('',(0.,-1.,0.));
#8585=DIRECTION('center_axis',(0.,1.,0.));
#8586=DIRECTION('ref_axis',(0.,0.,-1.));
#8587=DIRECTION('center_axis',(0.,-1.,0.));
#8588=DIRECTION('ref_axis',(0.,0.,-1.));
#8589=DIRECTION('center_axis',(0.,-1.,0.));
#8590=DIRECTION('ref_axis',(0.,0.,-1.));
#8591=DIRECTION('center_axis',(0.,-1.,0.));
#8592=DIRECTION('ref_axis',(0.,0.,-1.));
#8593=DIRECTION('',(0.,1.,0.));
#8594=DIRECTION('center_axis',(0.,-1.,0.));
#8595=DIRECTION('ref_axis',(0.,0.,1.));
#8596=DIRECTION('center_axis',(0.,-1.,0.));
#8597=DIRECTION('ref_axis',(0.,0.,-1.));
#8598=DIRECTION('center_axis',(0.,-1.,0.));
#8599=DIRECTION('ref_axis',(1.,0.,-1.75640751942652E-17));
#8600=DIRECTION('center_axis',(0.,0.,-1.));
#8601=DIRECTION('ref_axis',(-1.,0.,0.));
#8602=DIRECTION('',(0.,-1.,0.));
#8603=DIRECTION('',(0.,-1.,0.));
#8604=DIRECTION('center_axis',(0.,0.,1.));
#8605=DIRECTION('ref_axis',(0.,-1.,0.));
#8606=DIRECTION('center_axis',(0.,0.,1.));
#8607=DIRECTION('ref_axis',(0.,-1.,0.));
#8608=DIRECTION('',(0.,0.,1.));
#8609=DIRECTION('center_axis',(0.,0.,1.));
#8610=DIRECTION('ref_axis',(0.,-1.,0.));
#8611=DIRECTION('center_axis',(0.,0.,1.));
#8612=DIRECTION('ref_axis',(1.,0.,0.));
#8613=DIRECTION('',(0.,-1.,0.));
#8614=DIRECTION('center_axis',(0.,-1.,0.));
#8615=DIRECTION('ref_axis',(-1.,0.,-2.27465615787459E-16));
#8616=DIRECTION('center_axis',(0.,-1.,0.));
#8617=DIRECTION('ref_axis',(0.,0.,1.));
#8618=DIRECTION('',(0.,-1.,0.));
#8619=DIRECTION('center_axis',(0.,1.,0.));
#8620=DIRECTION('ref_axis',(-1.,0.,-1.22464679914735E-16));
#8621=DIRECTION('',(0.,-1.,0.));
#8622=DIRECTION('center_axis',(0.,-1.,0.));
#8623=DIRECTION('ref_axis',(-0.903507902905271,0.,-0.428571428571386));
#8624=DIRECTION('center_axis',(0.,-1.,0.));
#8625=DIRECTION('ref_axis',(0.,0.,-1.));
#8626=DIRECTION('',(0.,-1.,0.));
#8627=DIRECTION('center_axis',(0.,1.,0.));
#8628=DIRECTION('ref_axis',(1.,0.,0.));
#8629=DIRECTION('center_axis',(0.,-1.,0.));
#8630=DIRECTION('ref_axis',(1.,0.,0.));
#8631=DIRECTION('center_axis',(0.,-1.,0.));
#8632=DIRECTION('ref_axis',(-1.,0.,0.));
#8633=DIRECTION('',(0.,1.,0.));
#8634=DIRECTION('center_axis',(0.,-1.,0.));
#8635=DIRECTION('ref_axis',(-1.,0.,0.));
#8636=DIRECTION('center_axis',(0.,-1.,0.));
#8637=DIRECTION('ref_axis',(1.,0.,0.));
#8638=DIRECTION('center_axis',(0.,1.,0.));
#8639=DIRECTION('ref_axis',(-1.,0.,0.));
#8640=DIRECTION('axis',(0.,0.,1.));
#8641=DIRECTION('refdir',(1.,0.,0.));
#8642=DIRECTION('center_axis',(0.,1.,0.));
#8643=DIRECTION('ref_axis',(1.,0.,0.));
#8644=DIRECTION('center_axis',(0.,1.,0.));
#8645=DIRECTION('ref_axis',(1.,0.,0.));
#8646=DIRECTION('center_axis',(0.,-1.,0.));
#8647=DIRECTION('ref_axis',(0.,0.,-1.));
#8648=DIRECTION('center_axis',(0.,1.,0.));
#8649=DIRECTION('ref_axis',(1.,0.,0.));
#8650=DIRECTION('center_axis',(0.,1.,0.));
#8651=DIRECTION('ref_axis',(1.,0.,0.));
#8652=DIRECTION('',(0.,-1.,0.));
#8653=DIRECTION('center_axis',(0.,1.,0.));
#8654=DIRECTION('ref_axis',(1.,0.,0.));
#8655=DIRECTION('center_axis',(0.,-1.,0.));
#8656=DIRECTION('ref_axis',(0.,0.,-1.));
#8657=DIRECTION('center_axis',(0.,-1.,0.));
#8658=DIRECTION('ref_axis',(0.,0.,-1.));
#8659=DIRECTION('',(0.,1.,0.));
#8660=DIRECTION('center_axis',(0.,-1.,0.));
#8661=DIRECTION('ref_axis',(0.,0.,-1.));
#8662=DIRECTION('center_axis',(0.,-1.,0.));
#8663=DIRECTION('ref_axis',(1.,0.,0.));
#8664=DIRECTION('center_axis',(0.,-1.,0.));
#8665=DIRECTION('ref_axis',(-1.,0.,0.));
#8666=DIRECTION('',(0.,1.,0.));
#8667=DIRECTION('center_axis',(0.,-1.,0.));
#8668=DIRECTION('ref_axis',(-1.,0.,0.));
#8669=DIRECTION('center_axis',(0.,-1.,0.));
#8670=DIRECTION('ref_axis',(1.,0.,0.));
#8671=DIRECTION('center_axis',(0.,1.,0.));
#8672=DIRECTION('ref_axis',(-1.,0.,0.));
#8673=DIRECTION('center_axis',(0.,1.,0.));
#8674=DIRECTION('ref_axis',(-1.,0.,0.));
#8675=DIRECTION('center_axis',(0.,1.,0.));
#8676=DIRECTION('ref_axis',(1.,0.,0.));
#8677=DIRECTION('',(0.,-1.,0.));
#8678=DIRECTION('center_axis',(0.,1.,0.));
#8679=DIRECTION('ref_axis',(1.,0.,0.));
#8680=DIRECTION('center_axis',(0.,1.,0.));
#8681=DIRECTION('ref_axis',(-1.,0.,0.));
#8682=DIRECTION('center_axis',(0.,-1.,0.));
#8683=DIRECTION('ref_axis',(1.,0.,0.));
#8684=DIRECTION('axis',(0.,0.,1.));
#8685=DIRECTION('refdir',(1.,0.,0.));
#8686=DIRECTION('center_axis',(0.,0.,-1.));
#8687=DIRECTION('ref_axis',(0.,-1.,0.));
#8688=DIRECTION('center_axis',(0.,0.,1.));
#8689=DIRECTION('ref_axis',(0.,-1.,0.));
#8690=DIRECTION('center_axis',(0.,0.,-1.));
#8691=DIRECTION('ref_axis',(0.,-1.,0.));
#8692=DIRECTION('center_axis',(0.,0.,-1.));
#8693=DIRECTION('ref_axis',(0.,-1.,0.));
#8694=DIRECTION('',(0.,0.,-1.));
#8695=DIRECTION('center_axis',(0.,0.,-1.));
#8696=DIRECTION('ref_axis',(0.,-1.,0.));
#8697=DIRECTION('center_axis',(0.,0.,-1.));
#8698=DIRECTION('ref_axis',(0.,-1.,0.));
#8699=DIRECTION('center_axis',(0.,0.,-1.));
#8700=DIRECTION('ref_axis',(0.,-1.,0.));
#8701=DIRECTION('center_axis',(0.,0.,-1.));
#8702=DIRECTION('ref_axis',(0.,-1.,0.));
#8703=DIRECTION('',(0.,0.,1.));
#8704=DIRECTION('center_axis',(0.,0.,-1.));
#8705=DIRECTION('ref_axis',(0.,-1.,0.));
#8706=DIRECTION('center_axis',(0.,0.,-1.));
#8707=DIRECTION('ref_axis',(0.,-1.,0.));
#8708=DIRECTION('center_axis',(0.,0.,-1.));
#8709=DIRECTION('ref_axis',(0.,-1.,0.));
#8710=DIRECTION('center_axis',(0.,0.,-1.));
#8711=DIRECTION('ref_axis',(0.,-1.,0.));
#8712=DIRECTION('',(0.,0.,1.));
#8713=DIRECTION('center_axis',(0.,0.,-1.));
#8714=DIRECTION('ref_axis',(0.,-1.,0.));
#8715=DIRECTION('center_axis',(0.,0.,-1.));
#8716=DIRECTION('ref_axis',(0.,-1.,0.));
#8717=DIRECTION('center_axis',(0.,0.,-1.));
#8718=DIRECTION('ref_axis',(0.,-1.,0.));
#8719=DIRECTION('center_axis',(0.,0.,-1.));
#8720=DIRECTION('ref_axis',(0.,-1.,0.));
#8721=DIRECTION('',(0.,0.,1.));
#8722=DIRECTION('center_axis',(0.,0.,-1.));
#8723=DIRECTION('ref_axis',(-1.,0.,0.));
#8724=DIRECTION('center_axis',(0.,0.,-1.));
#8725=DIRECTION('ref_axis',(1.,0.,0.));
#8726=DIRECTION('',(0.,0.,1.));
#8727=DIRECTION('center_axis',(0.,0.,-1.));
#8728=DIRECTION('ref_axis',(1.,0.,0.));
#8729=DIRECTION('center_axis',(0.,0.,-1.));
#8730=DIRECTION('ref_axis',(-1.,0.,0.));
#8731=DIRECTION('center_axis',(0.,0.,1.));
#8732=DIRECTION('ref_axis',(1.,0.,0.));
#8733=DIRECTION('',(0.,0.,1.));
#8734=DIRECTION('',(1.,0.,0.));
#8735=DIRECTION('',(0.,0.,1.));
#8736=DIRECTION('',(1.,0.,0.));
#8737=DIRECTION('',(0.,1.,0.));
#8738=DIRECTION('',(1.,0.,0.));
#8739=DIRECTION('',(0.,0.,1.));
#8740=DIRECTION('',(1.,0.,0.));
#8741=DIRECTION('',(0.,1.,0.));
#8742=DIRECTION('',(1.,0.,0.));
#8743=DIRECTION('',(0.,0.,1.));
#8744=DIRECTION('',(0.,-1.,0.));
#8745=DIRECTION('',(1.,0.,0.));
#8746=DIRECTION('',(0.,0.,-1.));
#8747=DIRECTION('',(-1.,0.,0.));
#8748=DIRECTION('',(0.,1.,0.));
#8749=DIRECTION('axis',(0.,0.,1.));
#8750=DIRECTION('refdir',(1.,0.,0.));
#8751=DIRECTION('center_axis',(0.,0.,1.));
#8752=DIRECTION('ref_axis',(1.,0.,0.));
#8753=DIRECTION('center_axis',(0.,0.,1.));
#8754=DIRECTION('ref_axis',(0.,1.,0.));
#8755=DIRECTION('',(-1.,0.,0.));
#8756=DIRECTION('center_axis',(0.,0.,1.));
#8757=DIRECTION('ref_axis',(1.,0.,0.));
#8758=DIRECTION('',(0.,1.,0.));
#8759=DIRECTION('center_axis',(0.,0.,1.));
#8760=DIRECTION('ref_axis',(0.,-1.,0.));
#8761=DIRECTION('',(1.,0.,0.));
#8762=DIRECTION('center_axis',(0.,0.,1.));
#8763=DIRECTION('ref_axis',(-1.,0.,0.));
#8764=DIRECTION('',(0.,-1.,0.));
#8765=DIRECTION('center_axis',(0.,0.,-1.));
#8766=DIRECTION('ref_axis',(1.,0.,0.));
#8767=DIRECTION('center_axis',(0.,0.,-1.));
#8768=DIRECTION('ref_axis',(1.,0.,0.));
#8769=DIRECTION('center_axis',(0.,0.,1.));
#8770=DIRECTION('ref_axis',(1.,0.,0.));
#8771=DIRECTION('',(0.,0.,1.));
#8772=DIRECTION('center_axis',(0.,0.,1.));
#8773=DIRECTION('ref_axis',(-1.,0.,0.));
#8774=DIRECTION('center_axis',(0.,0.,1.));
#8775=DIRECTION('ref_axis',(1.,0.,0.));
#8776=DIRECTION('center_axis',(0.,0.,1.));
#8777=DIRECTION('ref_axis',(0.,1.,0.));
#8778=DIRECTION('',(0.,-1.,0.));
#8779=DIRECTION('center_axis',(0.,0.,1.));
#8780=DIRECTION('ref_axis',(-1.,0.,0.));
#8781=DIRECTION('',(1.,0.,0.));
#8782=DIRECTION('center_axis',(0.,0.,1.));
#8783=DIRECTION('ref_axis',(0.,-1.,0.));
#8784=DIRECTION('',(0.,1.,0.));
#8785=DIRECTION('center_axis',(0.,0.,1.));
#8786=DIRECTION('ref_axis',(1.,0.,0.));
#8787=DIRECTION('',(-1.,0.,0.));
#8788=DIRECTION('center_axis',(0.,0.,1.));
#8789=DIRECTION('ref_axis',(-1.,0.,0.));
#8790=DIRECTION('center_axis',(0.,0.,1.));
#8791=DIRECTION('ref_axis',(1.,0.,0.));
#8792=DIRECTION('center_axis',(0.,0.,1.));
#8793=DIRECTION('ref_axis',(0.,1.,0.));
#8794=DIRECTION('',(0.,0.,-1.));
#8795=DIRECTION('',(0.,0.,-1.));
#8796=DIRECTION('center_axis',(0.,0.,1.));
#8797=DIRECTION('ref_axis',(1.,0.,0.));
#8798=DIRECTION('center_axis',(0.,0.,1.));
#8799=DIRECTION('ref_axis',(0.,1.,0.));
#8800=DIRECTION('',(0.,-1.,0.));
#8801=DIRECTION('center_axis',(0.,0.,1.));
#8802=DIRECTION('ref_axis',(-1.,0.,0.));
#8803=DIRECTION('',(1.,0.,0.));
#8804=DIRECTION('center_axis',(0.,0.,1.));
#8805=DIRECTION('ref_axis',(0.,-1.,0.));
#8806=DIRECTION('',(0.,1.,0.));
#8807=DIRECTION('center_axis',(0.,0.,1.));
#8808=DIRECTION('ref_axis',(1.,0.,0.));
#8809=DIRECTION('',(-1.,0.,0.));
#8810=DIRECTION('',(-1.,0.,0.));
#8811=DIRECTION('center_axis',(0.,0.,1.));
#8812=DIRECTION('ref_axis',(1.,0.,0.));
#8813=DIRECTION('',(0.,1.,0.));
#8814=DIRECTION('center_axis',(0.,0.,1.));
#8815=DIRECTION('ref_axis',(0.,-1.,0.));
#8816=DIRECTION('',(1.,0.,0.));
#8817=DIRECTION('center_axis',(0.,0.,1.));
#8818=DIRECTION('ref_axis',(-1.,0.,0.));
#8819=DIRECTION('',(0.,-1.,0.));
#8820=DIRECTION('center_axis',(0.,0.,1.));
#8821=DIRECTION('ref_axis',(1.,0.,0.));
#8822=DIRECTION('',(0.,0.,1.));
#8823=DIRECTION('',(0.,0.,1.));
#8824=DIRECTION('center_axis',(0.,1.,0.));
#8825=DIRECTION('ref_axis',(-1.,0.,0.));
#8826=DIRECTION('',(0.,0.,1.));
#8827=DIRECTION('center_axis',(0.,0.,1.));
#8828=DIRECTION('ref_axis',(1.,0.,0.));
#8829=DIRECTION('',(0.,0.,1.));
#8830=DIRECTION('center_axis',(1.,0.,0.));
#8831=DIRECTION('ref_axis',(0.,1.,0.));
#8832=DIRECTION('',(0.,0.,1.));
#8833=DIRECTION('center_axis',(0.,0.,1.));
#8834=DIRECTION('ref_axis',(1.,0.,0.));
#8835=DIRECTION('',(0.,0.,1.));
#8836=DIRECTION('center_axis',(0.,-1.,0.));
#8837=DIRECTION('ref_axis',(1.,0.,0.));
#8838=DIRECTION('',(0.,0.,1.));
#8839=DIRECTION('center_axis',(0.,0.,1.));
#8840=DIRECTION('ref_axis',(1.,0.,0.));
#8841=DIRECTION('',(0.,0.,1.));
#8842=DIRECTION('center_axis',(-1.,0.,0.));
#8843=DIRECTION('ref_axis',(0.,-1.,0.));
#8844=DIRECTION('center_axis',(-1.,0.,0.));
#8845=DIRECTION('ref_axis',(0.,-1.,0.));
#8846=DIRECTION('',(0.,0.,-1.));
#8847=DIRECTION('center_axis',(0.,0.,1.));
#8848=DIRECTION('ref_axis',(1.,0.,0.));
#8849=DIRECTION('',(0.,0.,-1.));
#8850=DIRECTION('center_axis',(0.,-1.,0.));
#8851=DIRECTION('ref_axis',(1.,0.,0.));
#8852=DIRECTION('',(0.,0.,-1.));
#8853=DIRECTION('center_axis',(0.,0.,1.));
#8854=DIRECTION('ref_axis',(1.,0.,0.));
#8855=DIRECTION('',(0.,0.,-1.));
#8856=DIRECTION('center_axis',(1.,0.,0.));
#8857=DIRECTION('ref_axis',(0.,1.,0.));
#8858=DIRECTION('',(0.,0.,-1.));
#8859=DIRECTION('center_axis',(0.,0.,1.));
#8860=DIRECTION('ref_axis',(1.,0.,0.));
#8861=DIRECTION('',(0.,0.,-1.));
#8862=DIRECTION('center_axis',(0.,1.,0.));
#8863=DIRECTION('ref_axis',(-1.,0.,0.));
#8864=DIRECTION('center_axis',(0.,0.,1.));
#8865=DIRECTION('ref_axis',(1.,0.,0.));
#8866=DIRECTION('',(0.,0.,1.));
#8867=DIRECTION('',(0.,0.,1.));
#8868=DIRECTION('',(1.,0.,0.));
#8869=DIRECTION('',(0.,0.,1.));
#8870=DIRECTION('',(1.,0.,0.));
#8871=DIRECTION('',(0.783967454078606,-0.620801925694105,0.));
#8872=DIRECTION('',(0.620801925694105,0.783967454078606,0.));
#8873=DIRECTION('',(-0.203692616066002,-0.979034891186309,0.));
#8874=DIRECTION('',(0.,0.,-1.));
#8875=DIRECTION('',(8.1066450115199E-20,0.500000000000017,0.866025403784429));
#8876=DIRECTION('',(0.99999876993322,-0.00135834422570204,0.000784240404361284));
#8877=CARTESIAN_POINT('',(0.,0.,0.));
#8878=CARTESIAN_POINT('',(0.,0.,0.));
#8879=CARTESIAN_POINT('Origin',(0.,0.,-60.));
#8880=CARTESIAN_POINT('',(-50.,20.,-60.));
#8881=CARTESIAN_POINT('',(50.,20.,-60.));
#8882=CARTESIAN_POINT('',(-50.,20.,-60.));
#8883=CARTESIAN_POINT('',(50.,0.,-60.));
#8884=CARTESIAN_POINT('',(50.,0.,-60.));
#8885=CARTESIAN_POINT('',(-50.,0.,-60.));
#8886=CARTESIAN_POINT('',(-50.,0.,-60.));
#8887=CARTESIAN_POINT('',(-50.,20.,-60.));
#8888=CARTESIAN_POINT('Origin',(0.,22.5,-57.5));
#8889=CARTESIAN_POINT('',(-45.,25.,-55.));
#8890=CARTESIAN_POINT('',(-45.,25.,-55.));
#8891=CARTESIAN_POINT('',(45.,25.,-55.));
#8892=CARTESIAN_POINT('',(-45.,25.,-55.));
#8893=CARTESIAN_POINT('',(45.,25.,-55.));
#8894=CARTESIAN_POINT('Origin',(47.5,22.5,2.84217094304E-14));
#8895=CARTESIAN_POINT('',(45.,25.,47.87564434702));
#8896=CARTESIAN_POINT('',(50.,20.,50.76239569297));
#8897=CARTESIAN_POINT('',(45.,25.,47.87564434702));
#8898=CARTESIAN_POINT('',(50.,20.,50.76239569297));
#8899=CARTESIAN_POINT('',(45.,25.,47.87564434702));
#8900=CARTESIAN_POINT('Origin',(-57.3,4.,60.));
#8901=CARTESIAN_POINT('',(-50.,4.,60.));
#8902=CARTESIAN_POINT('',(50.,4.,60.));
#8903=CARTESIAN_POINT('',(-50.,4.,60.));
#8904=CARTESIAN_POINT('',(50.,20.,50.76239569297));
#8905=CARTESIAN_POINT('',(-45.,25.,47.87564434702));
#8906=CARTESIAN_POINT('',(45.,25.,47.87564434702));
#8907=CARTESIAN_POINT('',(-50.,20.,50.76239569297));
#8908=CARTESIAN_POINT('',(-50.,20.,50.76239569297));
#8909=CARTESIAN_POINT('',(-50.,20.,50.76239569297));
#8910=CARTESIAN_POINT('',(-27.5,14.17468245269,54.12564434702));
#8911=CARTESIAN_POINT('Origin',(-26.,14.17468245269,54.12564434702));
#8912=CARTESIAN_POINT('',(24.5,14.17468245269,54.12564434702));
#8913=CARTESIAN_POINT('Origin',(26.,14.17468245269,54.12564434702));
#8914=CARTESIAN_POINT('Origin',(0.,0.,60.));
#8915=CARTESIAN_POINT('',(-50.,0.,60.));
#8916=CARTESIAN_POINT('',(-50.,4.,60.));
#8917=CARTESIAN_POINT('',(50.,0.,60.));
#8918=CARTESIAN_POINT('',(-50.,0.,60.));
#8919=CARTESIAN_POINT('',(50.,0.,60.));
#8920=CARTESIAN_POINT('Origin',(50.,0.,-60.));
#8921=CARTESIAN_POINT('',(50.,0.,-60.));
#8922=CARTESIAN_POINT('Origin',(-50.,0.,-60.));
#8923=CARTESIAN_POINT('',(-50.,0.,-60.));
#8924=CARTESIAN_POINT('',(-32.5,0.,35.));
#8925=CARTESIAN_POINT('Origin',(-32.5,0.,32.5));
#8926=CARTESIAN_POINT('',(-32.5,0.,-30.));
#8927=CARTESIAN_POINT('Origin',(-32.5,0.,-32.5));
#8928=CARTESIAN_POINT('',(32.5,0.,35.));
#8929=CARTESIAN_POINT('Origin',(32.5,0.,32.5));
#8930=CARTESIAN_POINT('',(32.5,0.,-30.));
#8931=CARTESIAN_POINT('Origin',(32.5,0.,-32.5));
#8932=CARTESIAN_POINT('Origin',(-50.,25.,-60.));
#8933=CARTESIAN_POINT('',(-50.,20.,50.76239569297));
#8934=CARTESIAN_POINT('Origin',(-47.5,22.5,2.84217094304E-14));
#8935=CARTESIAN_POINT('',(-45.,25.,47.87564434702));
#8936=CARTESIAN_POINT('Origin',(50.,25.,-60.));
#8937=CARTESIAN_POINT('',(-32.5,25.,35.));
#8938=CARTESIAN_POINT('Origin',(-32.5,25.,32.5));
#8939=CARTESIAN_POINT('',(-32.5,25.,-30.));
#8940=CARTESIAN_POINT('Origin',(-32.5,25.,-32.5));
#8941=CARTESIAN_POINT('',(32.5,25.,35.));
#8942=CARTESIAN_POINT('Origin',(32.5,25.,32.5));
#8943=CARTESIAN_POINT('',(32.5,25.,-30.));
#8944=CARTESIAN_POINT('Origin',(32.5,25.,-32.5));
#8945=CARTESIAN_POINT('Origin',(-32.5,25.,32.5));
#8946=CARTESIAN_POINT('',(-32.5,25.,35.));
#8947=CARTESIAN_POINT('Origin',(-32.5,25.,-32.5));
#8948=CARTESIAN_POINT('',(-32.5,25.,-30.));
#8949=CARTESIAN_POINT('Origin',(32.5,25.,32.5));
#8950=CARTESIAN_POINT('',(32.5,25.,35.));
#8951=CARTESIAN_POINT('Origin',(32.5,25.,-32.5));
#8952=CARTESIAN_POINT('',(32.5,25.,-30.));
#8953=CARTESIAN_POINT('Origin',(-26.,14.17468245269,54.12564434702));
#8954=CARTESIAN_POINT('',(-27.5,9.17468245268864,45.4653903091737));
#8955=CARTESIAN_POINT('Origin',(-26.,9.174682452695,45.46539030917));
#8956=CARTESIAN_POINT('',(-27.5,14.17468245269,54.12564434702));
#8957=CARTESIAN_POINT('Origin',(-57.3,21.98076211353,38.07179676972));
#8958=CARTESIAN_POINT('Origin',(-57.3,21.98076211353,38.07179676972));
#8959=CARTESIAN_POINT('',(24.5,9.17468245268864,45.4653903091737));
#8960=CARTESIAN_POINT('Origin',(26.,9.174682452695,45.46539030917));
#8961=CARTESIAN_POINT('Origin',(26.,14.17468245269,54.12564434702));
#8962=CARTESIAN_POINT('',(24.5,14.17468245269,54.12564434702));
#8963=CARTESIAN_POINT('',(0.,0.,0.));
#8964=CARTESIAN_POINT('',(0.,0.,0.));
#8965=CARTESIAN_POINT('Origin',(0.,0.,0.));
#8966=CARTESIAN_POINT('',(-32.5,0.,-42.5));
#8967=CARTESIAN_POINT('',(-42.5,0.,-32.5));
#8968=CARTESIAN_POINT('Origin',(-32.5,0.,-32.5));
#8969=CARTESIAN_POINT('',(32.5,0.,-42.5));
#8970=CARTESIAN_POINT('',(32.5,0.,-42.5));
#8971=CARTESIAN_POINT('',(42.5,0.,-32.5));
#8972=CARTESIAN_POINT('Origin',(32.5,0.,-32.5));
#8973=CARTESIAN_POINT('',(42.5,0.,32.5));
#8974=CARTESIAN_POINT('',(42.5,0.,32.5));
#8975=CARTESIAN_POINT('',(32.5,0.,42.5));
#8976=CARTESIAN_POINT('Origin',(32.5,0.,32.5));
#8977=CARTESIAN_POINT('',(-32.5,0.,42.5));
#8978=CARTESIAN_POINT('',(-32.5,0.,42.5));
#8979=CARTESIAN_POINT('',(-42.5,0.,32.5));
#8980=CARTESIAN_POINT('Origin',(-32.5,0.,32.5));
#8981=CARTESIAN_POINT('',(-42.5,0.,-32.5));
#8982=CARTESIAN_POINT('',(-35.,0.,-32.5));
#8983=CARTESIAN_POINT('Origin',(-32.5,0.,-32.5));
#8984=CARTESIAN_POINT('',(30.,0.,32.5));
#8985=CARTESIAN_POINT('Origin',(32.5,0.,32.5));
#8986=CARTESIAN_POINT('',(30.,0.,-32.5));
#8987=CARTESIAN_POINT('Origin',(32.5,0.,-32.5));
#8988=CARTESIAN_POINT('',(13.25,0.,2.14313189850787E-16));
#8989=CARTESIAN_POINT('Origin',(15.,0.,0.));
#8990=CARTESIAN_POINT('',(-16.75,0.,2.14313189850787E-16));
#8991=CARTESIAN_POINT('Origin',(-15.,0.,0.));
#8992=CARTESIAN_POINT('',(-35.,0.,32.5));
#8993=CARTESIAN_POINT('Origin',(-32.5,0.,32.5));
#8994=CARTESIAN_POINT('Origin',(-32.5,0.,32.5));
#8995=CARTESIAN_POINT('',(-35.,6.,32.5));
#8996=CARTESIAN_POINT('',(-35.,0.,32.5));
#8997=CARTESIAN_POINT('Origin',(-32.5,6.,32.5));
#8998=CARTESIAN_POINT('Origin',(0.,6.,0.));
#8999=CARTESIAN_POINT('',(40.4999999999501,6.00000000004757,-32.4999999910564));
#9000=CARTESIAN_POINT('',(32.4999999901967,6.0000000000829,-40.4999999999151));
#9001=CARTESIAN_POINT('Origin',(32.5,6.,-32.5));
#9002=CARTESIAN_POINT('',(-32.4999999897,6.000000000096,-40.4999999999));
#9003=CARTESIAN_POINT('',(32.49999998871,6.000000000167,-40.49999999983));
#9004=CARTESIAN_POINT('',(-40.4999999999151,6.0000000000829,-32.4999999901967));
#9005=CARTESIAN_POINT('Origin',(-32.5,6.,-32.5));
#9006=CARTESIAN_POINT('',(-40.4999999999,6.000000000096,32.4999999897));
#9007=CARTESIAN_POINT('',(-40.49999999983,6.000000000167,-32.49999998871));
#9008=CARTESIAN_POINT('',(-32.4999999901967,6.0000000000829,40.4999999999151));
#9009=CARTESIAN_POINT('Origin',(-32.5,6.,32.5));
#9010=CARTESIAN_POINT('',(32.4999999897,6.000000000096,40.4999999999));
#9011=CARTESIAN_POINT('',(-32.49999998871,6.000000000167,40.49999999983));
#9012=CARTESIAN_POINT('',(40.4999999999151,6.0000000000829,32.4999999901967));
#9013=CARTESIAN_POINT('Origin',(32.5,6.,32.5));
#9014=CARTESIAN_POINT('',(40.49999999983,6.000000000167,32.49999998871));
#9015=CARTESIAN_POINT('',(-35.,6.,-32.5));
#9016=CARTESIAN_POINT('Origin',(-32.5,6.,-32.5));
#9017=CARTESIAN_POINT('',(30.,6.,32.5));
#9018=CARTESIAN_POINT('Origin',(32.5,6.,32.5));
#9019=CARTESIAN_POINT('',(30.,6.,-32.5));
#9020=CARTESIAN_POINT('Origin',(32.5,6.,-32.5));
#9021=CARTESIAN_POINT('',(13.25,6.,2.14313189850787E-16));
#9022=CARTESIAN_POINT('Origin',(15.,6.,0.));
#9023=CARTESIAN_POINT('',(-16.75,6.,2.14313189850787E-16));
#9024=CARTESIAN_POINT('Origin',(-15.,6.,0.));
#9025=CARTESIAN_POINT('Origin',(-32.5,0.,-32.5));
#9026=CARTESIAN_POINT('',(-35.,0.,-32.5));
#9027=CARTESIAN_POINT('Origin',(32.5,0.,32.5));
#9028=CARTESIAN_POINT('',(30.,0.,32.5));
#9029=CARTESIAN_POINT('Origin',(32.5,0.,-32.5));
#9030=CARTESIAN_POINT('',(30.,0.,-32.5));
#9031=CARTESIAN_POINT('Origin',(15.,0.,0.));
#9032=CARTESIAN_POINT('',(13.25,0.,2.14313189850787E-16));
#9033=CARTESIAN_POINT('Origin',(-15.,0.,0.));
#9034=CARTESIAN_POINT('',(-16.75,0.,2.14313189850787E-16));
#9035=CARTESIAN_POINT('Origin',(32.5,5.000000000251,-32.5));
#9036=CARTESIAN_POINT('',(42.4999999999408,4.00000000004547,-32.4999999909456));
#9037=CARTESIAN_POINT('',(40.4999999999,6.000000000096,-32.4999999897));
#9038=CARTESIAN_POINT('',(32.4999999900768,4.00000000007925,-42.4999999998988));
#9039=CARTESIAN_POINT('Origin',(32.5,4.,-32.5));
#9040=CARTESIAN_POINT('',(32.49999998871,6.000000000167,-40.49999999983));
#9041=CARTESIAN_POINT('Origin',(1.24344978758E-14,5.,-41.5));
#9042=CARTESIAN_POINT('',(-32.49999999034,4.00000000009,-42.49999999991));
#9043=CARTESIAN_POINT('',(32.49999998941,4.000000000157,-42.49999999984));
#9044=CARTESIAN_POINT('',(-32.4999999897,6.000000000096,-40.4999999999));
#9045=CARTESIAN_POINT('Origin',(-32.5,5.000000000251,-32.5));
#9046=CARTESIAN_POINT('',(-42.4999999998987,4.0000000000792,-32.4999999900768));
#9047=CARTESIAN_POINT('Origin',(-32.5,4.,-32.5));
#9048=CARTESIAN_POINT('',(-40.49999999983,6.000000000167,-32.49999998871));
#9049=CARTESIAN_POINT('Origin',(-41.5,5.,-1.24344978758E-14));
#9050=CARTESIAN_POINT('',(-42.49999999991,4.00000000009,32.49999999034));
#9051=CARTESIAN_POINT('',(-42.49999999984,4.000000000157,-32.49999998941));
#9052=CARTESIAN_POINT('',(-40.4999999999,6.000000000096,32.4999999897));
#9053=CARTESIAN_POINT('Origin',(-32.5,5.000000000251,32.5));
#9054=CARTESIAN_POINT('',(-32.4999999900768,4.00000000007925,42.4999999998988));
#9055=CARTESIAN_POINT('Origin',(-32.5,4.,32.5));
#9056=CARTESIAN_POINT('',(-32.49999998871,6.000000000167,40.49999999983));
#9057=CARTESIAN_POINT('Origin',(-1.24344978758E-14,5.,41.5));
#9058=CARTESIAN_POINT('',(32.49999999034,4.00000000009,42.49999999991));
#9059=CARTESIAN_POINT('',(-32.49999998941,4.000000000157,42.49999999984));
#9060=CARTESIAN_POINT('',(32.4999999897,6.000000000096,40.4999999999));
#9061=CARTESIAN_POINT('Origin',(32.5,5.000000000251,32.5));
#9062=CARTESIAN_POINT('',(42.4999999998987,4.0000000000792,32.4999999900768));
#9063=CARTESIAN_POINT('Origin',(32.5,4.,32.5));
#9064=CARTESIAN_POINT('',(40.49999999983,6.000000000167,32.49999998871));
#9065=CARTESIAN_POINT('Origin',(41.5,5.,1.24344978758E-14));
#9066=CARTESIAN_POINT('',(42.49999999984,4.000000000157,32.49999998941));
#9067=CARTESIAN_POINT('Origin',(42.5,0.,32.5));
#9068=CARTESIAN_POINT('',(42.5,0.,32.5));
#9069=CARTESIAN_POINT('',(42.5,0.,-32.5));
#9070=CARTESIAN_POINT('Origin',(32.5,0.,-32.5));
#9071=CARTESIAN_POINT('',(32.5,0.,-42.5));
#9072=CARTESIAN_POINT('Origin',(32.5,0.,-42.5));
#9073=CARTESIAN_POINT('',(-32.5,0.,-42.5));
#9074=CARTESIAN_POINT('Origin',(-32.5,0.,-32.5));
#9075=CARTESIAN_POINT('',(-42.5,0.,-32.5));
#9076=CARTESIAN_POINT('Origin',(-42.5,0.,-32.5));
#9077=CARTESIAN_POINT('',(-42.5,0.,32.5));
#9078=CARTESIAN_POINT('Origin',(-32.5,0.,32.5));
#9079=CARTESIAN_POINT('',(-32.5,0.,42.5));
#9080=CARTESIAN_POINT('Origin',(-32.5,0.,42.5));
#9081=CARTESIAN_POINT('',(32.5,0.,42.5));
#9082=CARTESIAN_POINT('Origin',(32.5,0.,32.5));
#9083=CARTESIAN_POINT('Origin',(-15.,6.,0.));
#9084=CARTESIAN_POINT('',(-13.,6.,-2.44929359829471E-16));
#9085=CARTESIAN_POINT('Origin',(-15.,6.,0.));
#9086=CARTESIAN_POINT('',(-13.,0.,-2.44929359829471E-16));
#9087=CARTESIAN_POINT('',(-13.,6.,-2.44929359829471E-16));
#9088=CARTESIAN_POINT('Origin',(-15.,0.,0.));
#9089=CARTESIAN_POINT('Origin',(-15.,0.,0.));
#9090=CARTESIAN_POINT('',(-16.75,0.,0.));
#9091=CARTESIAN_POINT('Origin',(-15.,0.,0.));
#9092=CARTESIAN_POINT('Origin',(15.,6.,0.));
#9093=CARTESIAN_POINT('',(17.,6.,-2.44929359829471E-16));
#9094=CARTESIAN_POINT('Origin',(15.,6.,0.));
#9095=CARTESIAN_POINT('',(17.,0.,-2.44929359829471E-16));
#9096=CARTESIAN_POINT('',(17.,6.,-2.44929359829471E-16));
#9097=CARTESIAN_POINT('Origin',(15.,0.,0.));
#9098=CARTESIAN_POINT('Origin',(15.,0.,0.));
#9099=CARTESIAN_POINT('',(13.25,0.,0.));
#9100=CARTESIAN_POINT('Origin',(15.,0.,0.));
#9101=CARTESIAN_POINT('',(0.,0.,0.));
#9102=CARTESIAN_POINT('Origin',(0.,0.,-7.));
#9103=CARTESIAN_POINT('',(-7.,116.,-7.));
#9104=CARTESIAN_POINT('',(7.,116.,-7.));
#9105=CARTESIAN_POINT('',(-7.,116.,-7.));
#9106=CARTESIAN_POINT('',(7.,102.,-7.));
#9107=CARTESIAN_POINT('',(7.,116.,-7.));
#9108=CARTESIAN_POINT('',(1.628604434127,101.999999999997,-7.));
#9109=CARTESIAN_POINT('',(7.,102.,-7.));
#9110=CARTESIAN_POINT('',(-1.628621699819,102.,-7.));
#9111=CARTESIAN_POINT('Ctrl Pts',(1.62860443416043,101.999999999993,-7.));
#9112=CARTESIAN_POINT('Ctrl Pts',(1.4853123590287,101.999999921671,-7.));
#9113=CARTESIAN_POINT('Ctrl Pts',(1.21253741465399,101.99898584252,-7.));
#9114=CARTESIAN_POINT('Ctrl Pts',(0.8573044679824,101.9969182521,-7.));
#9115=CARTESIAN_POINT('Ctrl Pts',(0.5185327144029,101.9951338414,-7.));
#9116=CARTESIAN_POINT('Ctrl Pts',(0.1644709951681,101.9940222806,-7.));
#9117=CARTESIAN_POINT('Ctrl Pts',(-0.2218799388119,101.9940840565,-7.));
#9118=CARTESIAN_POINT('Ctrl Pts',(-0.6437910911378,101.9956599723,-7.));
#9119=CARTESIAN_POINT('Ctrl Pts',(-1.107253407488,101.998441137,-7.));
#9120=CARTESIAN_POINT('Ctrl Pts',(-1.449586300965,101.9999999758,-7.));
#9121=CARTESIAN_POINT('Ctrl Pts',(-1.628621699819,102.,-7.));
#9122=CARTESIAN_POINT('',(-7.,102.,-7.));
#9123=CARTESIAN_POINT('',(-1.628621699819,102.,-7.));
#9124=CARTESIAN_POINT('',(-7.,102.,-7.));
#9125=CARTESIAN_POINT('',(-4.5,109.,-7.));
#9126=CARTESIAN_POINT('Origin',(0.,109.,-7.));
#9127=CARTESIAN_POINT('Origin',(0.,109.,-7.));
#9128=CARTESIAN_POINT('',(-4.5,109.,-11.));
#9129=CARTESIAN_POINT('',(-4.5,109.,-7.));
#9130=CARTESIAN_POINT('',(4.49469945356788,109.218350228066,-11.));
#9131=CARTESIAN_POINT('Origin',(0.,109.,-11.));
#9132=CARTESIAN_POINT('Origin',(0.,109.,-11.));
#9133=CARTESIAN_POINT('Origin',(0.,109.,-11.));
#9134=CARTESIAN_POINT('',(3.99528840317145,109.194089091614,-11.5));
#9135=CARTESIAN_POINT('Origin',(3.99528840317145,109.194089091614,-11.));
#9136=CARTESIAN_POINT('Origin',(0.,109.,-11.5));
#9137=CARTESIAN_POINT('Origin',(0.,0.,-11.5));
#9138=CARTESIAN_POINT('',(-2.5,109.,-11.5));
#9139=CARTESIAN_POINT('Origin',(0.,109.,-11.5));
#9140=CARTESIAN_POINT('Origin',(0.,109.,11.5));
#9141=CARTESIAN_POINT('',(-2.5,109.,11.5));
#9142=CARTESIAN_POINT('',(-2.5,109.,11.5));
#9143=CARTESIAN_POINT('Origin',(0.,109.,11.5));
#9144=CARTESIAN_POINT('',(1.25,111.1650635095,0.));
#9145=CARTESIAN_POINT('',(-1.25,111.165063509461,1.53080849893419E-16));
#9146=CARTESIAN_POINT('Ctrl Pts',(1.25,111.165063509461,1.04083408558608E-16));
#9147=CARTESIAN_POINT('Ctrl Pts',(1.25,111.165063509461,-0.160381333700613));
#9148=CARTESIAN_POINT('Ctrl Pts',(1.21735698059595,111.184781794941,-0.32892325157911));
#9149=CARTESIAN_POINT('Ctrl Pts',(1.08903588717028,111.251495015576,-0.635727949384779));
#9150=CARTESIAN_POINT('Ctrl Pts',(0.993444785163793,111.297125584436,-0.774322167802576));
#9151=CARTESIAN_POINT('Ctrl Pts',(0.774620837257829,111.379833262588,-0.993146115708541));
#9152=CARTESIAN_POINT('Ctrl Pts',(0.635925947642968,111.422831051299,-1.08895634990573));
#9153=CARTESIAN_POINT('Ctrl Pts',(0.328681344361066,111.483239960438,-1.21745488233641));
#9154=CARTESIAN_POINT('Ctrl Pts',(0.159944126385861,111.5,-1.25));
#9155=CARTESIAN_POINT('Ctrl Pts',(-0.159944126385861,111.5,-1.25));
#9156=CARTESIAN_POINT('Ctrl Pts',(-0.328681344361067,111.483239960438,-1.21745488233641));
#9157=CARTESIAN_POINT('Ctrl Pts',(-0.635925947642968,111.422831051299,-1.08895634990573));
#9158=CARTESIAN_POINT('Ctrl Pts',(-0.774620837257829,111.379833262588,-0.993146115708541));
#9159=CARTESIAN_POINT('Ctrl Pts',(-0.993444785163793,111.297125584436,-0.774322167802577));
#9160=CARTESIAN_POINT('Ctrl Pts',(-1.08903588717028,111.251495015576,-0.63572794938478));
#9161=CARTESIAN_POINT('Ctrl Pts',(-1.21735698059595,111.184781794941,-0.328923251579112));
#9162=CARTESIAN_POINT('Ctrl Pts',(-1.25,111.165063509461,-0.160381333700614));
#9163=CARTESIAN_POINT('Ctrl Pts',(-1.25,111.165063509461,-3.46944695195361E-16));
#9164=CARTESIAN_POINT('Ctrl Pts',(-1.25,111.165063509461,2.77555756156289E-16));
#9165=CARTESIAN_POINT('Ctrl Pts',(-1.25,111.165063509461,0.160381333700614));
#9166=CARTESIAN_POINT('Ctrl Pts',(-1.21735698059595,111.184781794941,0.328923251579112));
#9167=CARTESIAN_POINT('Ctrl Pts',(-1.08903588717028,111.251495015576,0.63572794938478));
#9168=CARTESIAN_POINT('Ctrl Pts',(-0.993444785163793,111.297125584436,0.774322167802577));
#9169=CARTESIAN_POINT('Ctrl Pts',(-0.774620837257829,111.379833262588,0.993146115708541));
#9170=CARTESIAN_POINT('Ctrl Pts',(-0.635925947642968,111.422831051299,1.08895634990573));
#9171=CARTESIAN_POINT('Ctrl Pts',(-0.328681344361067,111.483239960438,1.21745488233641));
#9172=CARTESIAN_POINT('Ctrl Pts',(-0.159944126385861,111.5,1.25));
#9173=CARTESIAN_POINT('Ctrl Pts',(0.159944126385861,111.5,1.25));
#9174=CARTESIAN_POINT('Ctrl Pts',(0.328681344361067,111.483239960438,1.21745488233641));
#9175=CARTESIAN_POINT('Ctrl Pts',(0.635925947642968,111.422831051299,1.08895634990573));
#9176=CARTESIAN_POINT('Ctrl Pts',(0.774620837257829,111.379833262588,0.993146115708541));
#9177=CARTESIAN_POINT('Ctrl Pts',(0.993444785163793,111.297125584436,0.774322167802577));
#9178=CARTESIAN_POINT('Ctrl Pts',(1.08903588717028,111.251495015576,0.635727949384779));
#9179=CARTESIAN_POINT('Ctrl Pts',(1.21735698059595,111.184781794941,0.32892325157911));
#9180=CARTESIAN_POINT('Ctrl Pts',(1.25,111.165063509461,0.160381333700614));
#9181=CARTESIAN_POINT('Ctrl Pts',(1.25,111.165063509461,4.33680868994202E-16));
#9182=CARTESIAN_POINT('Origin',(0.,0.,11.5));
#9183=CARTESIAN_POINT('',(3.99766495829864,108.863343931012,11.5));
#9184=CARTESIAN_POINT('Origin',(0.,109.,11.5));
#9185=CARTESIAN_POINT('Origin',(0.,109.,11.));
#9186=CARTESIAN_POINT('',(4.49737307808597,108.846261922389,11.));
#9187=CARTESIAN_POINT('Origin',(3.99766495829864,108.863343931012,11.));
#9188=CARTESIAN_POINT('',(-4.5,109.,11.));
#9189=CARTESIAN_POINT('Origin',(0.,109.,11.));
#9190=CARTESIAN_POINT('Origin',(0.,109.,11.));
#9191=CARTESIAN_POINT('Origin',(0.,109.,7.));
#9192=CARTESIAN_POINT('',(-4.5,109.,7.));
#9193=CARTESIAN_POINT('',(-4.5,109.,7.));
#9194=CARTESIAN_POINT('Origin',(0.,109.,7.));
#9195=CARTESIAN_POINT('Origin',(0.,0.,7.));
#9196=CARTESIAN_POINT('',(7.,102.,7.));
#9197=CARTESIAN_POINT('',(7.,116.,7.));
#9198=CARTESIAN_POINT('',(7.,102.,7.));
#9199=CARTESIAN_POINT('',(-7.,116.,7.));
#9200=CARTESIAN_POINT('',(7.,116.,7.));
#9201=CARTESIAN_POINT('',(-7.,102.,7.));
#9202=CARTESIAN_POINT('',(-7.,116.,7.));
#9203=CARTESIAN_POINT('',(-1.628604434127,101.999999999997,7.));
#9204=CARTESIAN_POINT('',(-7.,102.,7.));
#9205=CARTESIAN_POINT('',(1.628621699819,102.,7.));
#9206=CARTESIAN_POINT('Ctrl Pts',(-1.62860443416043,101.999999999993,7.));
#9207=CARTESIAN_POINT('Ctrl Pts',(-1.4853123590287,101.999999921671,7.));
#9208=CARTESIAN_POINT('Ctrl Pts',(-1.21253741465399,101.99898584252,7.));
#9209=CARTESIAN_POINT('Ctrl Pts',(-0.8573044679823,101.9969182521,7.));
#9210=CARTESIAN_POINT('Ctrl Pts',(-0.5185327144029,101.9951338414,7.));
#9211=CARTESIAN_POINT('Ctrl Pts',(-0.1644709951681,101.9940222806,7.));
#9212=CARTESIAN_POINT('Ctrl Pts',(0.2218799388119,101.9940840565,7.));
#9213=CARTESIAN_POINT('Ctrl Pts',(0.6437910911378,101.9956599723,7.));
#9214=CARTESIAN_POINT('Ctrl Pts',(1.107253407488,101.998441137,7.));
#9215=CARTESIAN_POINT('Ctrl Pts',(1.449586300965,101.9999999758,7.));
#9216=CARTESIAN_POINT('Ctrl Pts',(1.628621699819,102.,7.));
#9217=CARTESIAN_POINT('',(1.628621699819,102.,7.));
#9218=CARTESIAN_POINT('Origin',(7.,-143.7058229487,6.));
#9219=CARTESIAN_POINT('',(8.,102.,6.));
#9220=CARTESIAN_POINT('',(8.,116.,6.));
#9221=CARTESIAN_POINT('',(8.,102.,6.));
#9222=CARTESIAN_POINT('Origin',(7.,116.,6.));
#9223=CARTESIAN_POINT('Origin',(7.,102.,6.));
#9224=CARTESIAN_POINT('Origin',(8.,101.,-7.));
#9225=CARTESIAN_POINT('',(8.,102.,-6.));
#9226=CARTESIAN_POINT('',(8.,102.,6.));
#9227=CARTESIAN_POINT('',(8.,116.,-6.));
#9228=CARTESIAN_POINT('',(8.,116.,-6.));
#9229=CARTESIAN_POINT('',(8.,116.,6.));
#9230=CARTESIAN_POINT('Origin',(7.,102.,43.78380184031));
#9231=CARTESIAN_POINT('',(7.,101.,6.));
#9232=CARTESIAN_POINT('Origin',(7.,102.,6.));
#9233=CARTESIAN_POINT('',(7.,101.,-6.));
#9234=CARTESIAN_POINT('',(7.,101.,6.));
#9235=CARTESIAN_POINT('Origin',(7.,102.,-6.));
#9236=CARTESIAN_POINT('Origin',(7.,102.,-6.));
#9237=CARTESIAN_POINT('Origin',(7.,102.,-6.));
#9238=CARTESIAN_POINT('Origin',(7.,102.,-6.));
#9239=CARTESIAN_POINT('Origin',(75.7512,102.,-6.));
#9240=CARTESIAN_POINT('',(1.62860689419666,100.999999999996,-6.00000151345914));
#9241=CARTESIAN_POINT('',(7.,101.,-6.));
#9242=CARTESIAN_POINT('Origin',(1.628604434127,102.,-6.));
#9243=CARTESIAN_POINT('Ctrl Pts',(1.689481893123,102.1196847108,-6.992808061201));
#9244=CARTESIAN_POINT('Ctrl Pts',(1.669187233917,102.1197065598,-6.992808061201));
#9245=CARTESIAN_POINT('Ctrl Pts',(1.512636201126,102.1197869626,-6.992808061201));
#9246=CARTESIAN_POINT('Ctrl Pts',(1.23556503978,102.1188276871,-6.992808061201));
#9247=CARTESIAN_POINT('Ctrl Pts',(0.8648101546223,102.1166806136,-6.992808061201));
#9248=CARTESIAN_POINT('Ctrl Pts',(0.5109811635092,102.1148120947,-6.992808061201));
#9249=CARTESIAN_POINT('Ctrl Pts',(0.1488522802808,102.1137128273,-6.992808061201));
#9250=CARTESIAN_POINT('Ctrl Pts',(-0.2394130054686,102.1138378158,-6.992808061201));
#9251=CARTESIAN_POINT('Ctrl Pts',(-0.663639050088,102.1154833678,-6.992808061201));
#9252=CARTESIAN_POINT('Ctrl Pts',(-1.130096203131,102.1183003163,-6.992808061201));
#9253=CARTESIAN_POINT('Ctrl Pts',(-1.477116016106,102.1198046106,-6.992808061201));
#9254=CARTESIAN_POINT('Ctrl Pts',(-1.669209716084,102.1197066226,-6.992808061201));
#9255=CARTESIAN_POINT('Ctrl Pts',(-1.689515664192,102.1196849348,-6.992808061201));
#9256=CARTESIAN_POINT('Ctrl Pts',(1.688715228218,101.4207068678,-7.077093790264));
#9257=CARTESIAN_POINT('Ctrl Pts',(1.668689128932,101.4207284853,-7.077093790264));
#9258=CARTESIAN_POINT('Ctrl Pts',(1.514109227167,101.4208080916,-7.077093790264));
#9259=CARTESIAN_POINT('Ctrl Pts',(1.239188923109,101.4198586149,-7.077093790264));
#9260=CARTESIAN_POINT('Ctrl Pts',(0.8689370512759,101.41771466,-7.077093790264));
#9261=CARTESIAN_POINT('Ctrl Pts',(0.5140416525734,101.4158400361,-7.077093790264));
#9262=CARTESIAN_POINT('Ctrl Pts',(0.1498433242845,101.4147339759,-7.077093790264));
#9263=CARTESIAN_POINT('Ctrl Pts',(-0.2409905058727,101.4148598525,-7.077093790264));
#9264=CARTESIAN_POINT('Ctrl Pts',(-0.667428084141,101.4165149357,-7.077093790264));
#9265=CARTESIAN_POINT('Ctrl Pts',(-1.134325060388,101.4193353122,-7.077093790264));
#9266=CARTESIAN_POINT('Ctrl Pts',(-1.479036591025,101.4208256727,-7.077093790264));
#9267=CARTESIAN_POINT('Ctrl Pts',(-1.668711295896,101.4207285315,-7.077093790264));
#9268=CARTESIAN_POINT('Ctrl Pts',(-1.688748453112,101.4207070467,-7.077093790264));
#9269=CARTESIAN_POINT('Ctrl Pts',(1.68816918717,100.9228745154,-6.579261201271));
#9270=CARTESIAN_POINT('Ctrl Pts',(1.668334364073,100.922895968,-6.579261201271));
#9271=CARTESIAN_POINT('Ctrl Pts',(1.515158359163,100.9229750071,-6.579261201271));
#9272=CARTESIAN_POINT('Ctrl Pts',(1.241769958231,100.9220325094,-6.579261201271));
#9273=CARTESIAN_POINT('Ctrl Pts',(0.8718763471198,100.9198907756,-6.579261201271));
#9274=CARTESIAN_POINT('Ctrl Pts',(0.5162214219116,100.9180118035,-6.579261201271));
#9275=CARTESIAN_POINT('Ctrl Pts',(0.1505491746524,100.9169009054,-6.579261201271));
#9276=CARTESIAN_POINT('Ctrl Pts',(-0.2421140475483,100.9170274144,-6.579261201271));
#9277=CARTESIAN_POINT('Ctrl Pts',(-0.6701267444128,100.918689286,-6.579261201271));
#9278=CARTESIAN_POINT('Ctrl Pts',(-1.137336975539,100.9215121041,-6.579261201271));
#9279=CARTESIAN_POINT('Ctrl Pts',(-1.480404480349,100.9229925405,-6.579261201271));
#9280=CARTESIAN_POINT('Ctrl Pts',(-1.668356306539,100.9228960023,-6.579261201271));
#9281=CARTESIAN_POINT('Ctrl Pts',(-1.688202023064,100.9228746621,-6.579261201271));
#9282=CARTESIAN_POINT('Ctrl Pts',(1.688261634851,101.0071602049,-5.880283026469));
#9283=CARTESIAN_POINT('Ctrl Pts',(1.668394427668,101.0071816854,-5.880283026469));
#9284=CARTESIAN_POINT('Ctrl Pts',(1.514980735485,101.0072608205,-5.880283026469));
#9285=CARTESIAN_POINT('Ctrl Pts',(1.241332975131,101.0063171412,-5.880283026469));
#9286=CARTESIAN_POINT('Ctrl Pts',(0.8713787085563,101.0041750314,-5.880283026469));
#9287=CARTESIAN_POINT('Ctrl Pts',(0.5158523752623,101.0022967954,-5.880283026469));
#9288=CARTESIAN_POINT('Ctrl Pts',(0.1504296703963,101.0011867164,-5.880283026469));
#9289=CARTESIAN_POINT('Ctrl Pts',(-0.2419238259118,101.0013131184,-5.880283026469));
#9290=CARTESIAN_POINT('Ctrl Pts',(-0.6696698467433,101.0029738406,-5.880283026469));
#9291=CARTESIAN_POINT('Ctrl Pts',(-1.136827042137,101.0057962454,-5.880283026469));
#9292=CARTESIAN_POINT('Ctrl Pts',(-1.480172889344,101.007278362,-5.880283026469));
#9293=CARTESIAN_POINT('Ctrl Pts',(-1.668416408143,101.0071817217,-5.880283026469));
#9294=CARTESIAN_POINT('Ctrl Pts',(-1.688294536604,101.007160357,-5.880283026469));
#9295=CARTESIAN_POINT('',(-1.62862169826789,100.999999999995,-5.99999999986848));
#9296=CARTESIAN_POINT('Ctrl Pts',(1.62860685825195,100.999999999983,-6.0000009545634));
#9297=CARTESIAN_POINT('Ctrl Pts',(1.52373488016319,100.99999997304,-6.00674566973353));
#9298=CARTESIAN_POINT('Ctrl Pts',(1.42263846185517,100.99978700057,-6.01267762823953));
#9299=CARTESIAN_POINT('Ctrl Pts',(1.32582463231981,100.999497837555,-6.01787098237482));
#9300=CARTESIAN_POINT('Ctrl Pts',(1.29209674790815,100.999397099295,-6.01968023678428));
#9301=CARTESIAN_POINT('Ctrl Pts',(1.25888843888297,100.999286698235,-6.02139992825534));
#9302=CARTESIAN_POINT('Ctrl Pts',(1.22622051364658,100.999171092663,-6.02303342418429));
#9303=CARTESIAN_POINT('Ctrl Pts',(1.13537596273316,100.998849611083,-6.02757592888917));
#9304=CARTESIAN_POINT('Ctrl Pts',(1.04870946239408,100.998489638665,-6.03145127898147));
#9305=CARTESIAN_POINT('Ctrl Pts',(0.964146579740458,100.998135827758,-6.03481770912858));
#9306=CARTESIAN_POINT('Ctrl Pts',(0.931009084803032,100.997997180556,-6.03613690566559));
#9307=CARTESIAN_POINT('Ctrl Pts',(0.898194045077884,100.997859230698,-6.03737801560314));
#9308=CARTESIAN_POINT('Ctrl Pts',(0.865574716854578,100.997724090006,-6.03855077139743));
#9309=CARTESIAN_POINT('Ctrl Pts',(0.763673785219037,100.997301918145,-6.04221439399569));
#9310=CARTESIAN_POINT('Ctrl Pts',(0.663692099762057,100.996905553624,-6.04521010595944));
#9311=CARTESIAN_POINT('Ctrl Pts',(0.562039110946944,100.996569111419,-6.04760859093508));
#9312=CARTESIAN_POINT('Ctrl Pts',(0.548114095188321,100.996523023615,-6.04793714931268));
#9313=CARTESIAN_POINT('Ctrl Pts',(0.534157650522232,100.996478102747,-6.04825450644789));
#9314=CARTESIAN_POINT('Ctrl Pts',(0.520160493462915,100.996434487254,-6.04856084923628));
#9315=CARTESIAN_POINT('Ctrl Pts',(0.412198444871786,100.996098074806,-6.05092371441429));
#9316=CARTESIAN_POINT('Ctrl Pts',(0.301819293815625,100.995835695599,-6.0526309202976));
#9317=CARTESIAN_POINT('Ctrl Pts',(0.186840756394499,100.995693614002,-6.05353748689817));
#9318=CARTESIAN_POINT('Ctrl Pts',(0.178092147645217,100.995682803147,-6.05360646669798));
#9319=CARTESIAN_POINT('Ctrl Pts',(0.169316919910494,100.995672713175,-6.05367081239838));
#9320=CARTESIAN_POINT('Ctrl Pts',(0.160514117704065,100.995663377513,-6.05373046080016));
#9321=CARTESIAN_POINT('Ctrl Pts',(0.0496839098288051,100.995545838423,-6.05448145401959));
#9322=CARTESIAN_POINT('Ctrl Pts',(-0.0655181192494277,100.995546458708,
-6.05448756792474));
#9323=CARTESIAN_POINT('Ctrl Pts',(-0.185310647992566,100.995691809128,-6.05354829979092));
#9324=CARTESIAN_POINT('Ctrl Pts',(-0.200078909707018,100.995709728218,-6.05343250494323));
#9325=CARTESIAN_POINT('Ctrl Pts',(-0.214916879107109,100.995729871175,-6.05330234750083));
#9326=CARTESIAN_POINT('Ctrl Pts',(-0.229824912171414,100.995752309851,-6.05315745718398));
#9327=CARTESIAN_POINT('Ctrl Pts',(-0.340529448807116,100.995918935677,-6.05208152615263));
#9328=CARTESIAN_POINT('Ctrl Pts',(-0.455099630540629,100.996212269576,-6.0501929592695));
#9329=CARTESIAN_POINT('Ctrl Pts',(-0.573986781723262,100.996609420841,-6.04732336142487));
#9330=CARTESIAN_POINT('Ctrl Pts',(-0.600974002364567,100.996699573634,-6.0466719666407));
#9331=CARTESIAN_POINT('Ctrl Pts',(-0.628183462748757,100.996795071311,-6.04597004841208));
#9332=CARTESIAN_POINT('Ctrl Pts',(-0.655620049589773,100.996895635329,-6.04521569132264));
#9333=CARTESIAN_POINT('Ctrl Pts',(-0.764243748505043,100.997293776528,-6.04222912969847));
#9334=CARTESIAN_POINT('Ctrl Pts',(-0.87642962165337,100.997773482976,-6.0384203844328));
#9335=CARTESIAN_POINT('Ctrl Pts',(-0.99232222130473,100.998254098085,-6.0336721558827));
#9336=CARTESIAN_POINT('Ctrl Pts',(-1.03465714845761,100.998429664132,-6.03193765419426));
#9337=CARTESIAN_POINT('Ctrl Pts',(-1.07748630376386,100.998605095003,-6.03007786532948));
#9338=CARTESIAN_POINT('Ctrl Pts',(-1.1208152583269,100.998775489421,-6.02808737922741));
#9339=CARTESIAN_POINT('Ctrl Pts',(-1.22117671474146,100.999170168501,-6.02347688063145));
#9340=CARTESIAN_POINT('Ctrl Pts',(-1.32422004237134,100.999540506896,-6.01816518674119));
#9341=CARTESIAN_POINT('Ctrl Pts',(-1.43019217801676,100.999770783872,-6.01208235725501));
#9342=CARTESIAN_POINT('Ctrl Pts',(-1.49521612659923,100.999912080621,-6.00834996487341));
#9343=CARTESIAN_POINT('Ctrl Pts',(-1.56134223689861,101.00000001874,-6.00432736857725));
#9344=CARTESIAN_POINT('Ctrl Pts',(-1.628621697537,100.999999999981,-5.999999999856));
#9345=CARTESIAN_POINT('Origin',(-1.628621700447,102.,-6.));
#9346=CARTESIAN_POINT('Origin',(8.147852,102.,-6.));
#9347=CARTESIAN_POINT('',(-7.,101.,-6.));
#9348=CARTESIAN_POINT('',(-1.628621697537,101.,-5.999999999856));
#9349=CARTESIAN_POINT('Origin',(-7.,102.,-6.));
#9350=CARTESIAN_POINT('Origin',(-8.,101.,-7.));
#9351=CARTESIAN_POINT('',(1.62862169826789,101.,5.99999999986848));
#9352=CARTESIAN_POINT('',(1.628621697537,101.,5.999999999856));
#9353=CARTESIAN_POINT('',(6.21170021154708,101.,-0.259208631163567));
#9354=CARTESIAN_POINT('Origin',(0.,101.,0.));
#9355=CARTESIAN_POINT('Origin',(0.,101.,0.));
#9356=CARTESIAN_POINT('Origin',(-8.,101.,-7.));
#9357=CARTESIAN_POINT('',(-1.62860689419665,101.,6.00000151345915));
#9358=CARTESIAN_POINT('Origin',(0.,101.,0.));
#9359=CARTESIAN_POINT('',(-7.,101.,6.));
#9360=CARTESIAN_POINT('',(-7.,101.,6.));
#9361=CARTESIAN_POINT('',(-7.,101.,6.));
#9362=CARTESIAN_POINT('Origin',(0.,98.,0.));
#9363=CARTESIAN_POINT('',(3.22161027626912,97.79073057877,-0.134434882788108));
#9364=CARTESIAN_POINT('Origin',(6.21170021154708,98.,-0.259208631163567));
#9365=CARTESIAN_POINT('',(3.22441397929396,97.7907305787699,3.94876825886832E-16));
#9366=CARTESIAN_POINT('Origin',(0.,97.79073057877,0.));
#9367=CARTESIAN_POINT('Origin',(0.,97.79073057877,0.));
#9368=CARTESIAN_POINT('Ctrl Pts',(-1.62860685825194,100.999999999999,6.00000095456346));
#9369=CARTESIAN_POINT('Ctrl Pts',(-1.5402385437957,100.999999982535,6.00568425715639));
#9370=CARTESIAN_POINT('Ctrl Pts',(-1.45455562762397,100.999846865067,6.01079408210886));
#9371=CARTESIAN_POINT('Ctrl Pts',(-1.3718508879526,100.999627223085,6.01536640130176));
#9372=CARTESIAN_POINT('Ctrl Pts',(-1.32221134199258,100.99949539354,6.01811071619376));
#9373=CARTESIAN_POINT('Ctrl Pts',(-1.27364518931805,100.999338908544,6.02066204596849));
#9374=CARTESIAN_POINT('Ctrl Pts',(-1.22622051364658,100.999171092663,6.02303342418429));
#9375=CARTESIAN_POINT('Ctrl Pts',(-1.17181301863647,100.998978567536,6.02575396463326));
#9376=CARTESIAN_POINT('Ctrl Pts',(-1.11890846799787,100.998770692355,6.02821724570366));
#9377=CARTESIAN_POINT('Ctrl Pts',(-1.06705384911434,100.998560015031,6.03048981059644));
#9378=CARTESIAN_POINT('Ctrl Pts',(-1.01372995415689,100.998343368265,6.03282676753944));
#9379=CARTESIAN_POINT('Ctrl Pts',(-0.961516257209871,100.998123681242,6.03496189854049));
#9380=CARTESIAN_POINT('Ctrl Pts',(-0.909929062859923,100.997908538361,6.03691381376813));
#9381=CARTESIAN_POINT('Ctrl Pts',(-0.895096211312916,100.997846678389,6.037475047407));
#9382=CARTESIAN_POINT('Ctrl Pts',(-0.880315213774708,100.99778516074,6.0380208093818));
#9383=CARTESIAN_POINT('Ctrl Pts',(-0.865574716854661,100.997724089988,6.03855077139813));
#9384=CARTESIAN_POINT('Ctrl Pts',(-0.812672184995172,100.997504911662,6.04045276511006));
#9385=CARTESIAN_POINT('Ctrl Pts',(-0.760288018369843,100.997291776737,6.04215834916175));
#9386=CARTESIAN_POINT('Ctrl Pts',(-0.707917910975415,100.997091119445,6.0437082383946));
#9387=CARTESIAN_POINT('Ctrl Pts',(-0.655517128523072,100.996890344621,6.04525903545339));
#9388=CARTESIAN_POINT('Ctrl Pts',(-0.603130360414094,100.996702033618,6.04665393791658));
#9389=CARTESIAN_POINT('Ctrl Pts',(-0.550254983870303,100.996530278855,6.0478819218511));
#9390=CARTESIAN_POINT('Ctrl Pts',(-0.540242132749313,100.996497754172,6.04811446147765));
#9391=CARTESIAN_POINT('Ctrl Pts',(-0.530211769198876,100.996465817122,6.04834086581166));
#9392=CARTESIAN_POINT('Ctrl Pts',(-0.52016049346279,100.996434487268,6.04856084923561));
#9393=CARTESIAN_POINT('Ctrl Pts',(-0.4591600625234,100.996244348761,6.04989591196922));
#9394=CARTESIAN_POINT('Ctrl Pts',(-0.397386423926234,100.996077279975,6.0510104023759));
#9395=CARTESIAN_POINT('Ctrl Pts',(-0.334449136934581,100.995942794773,6.05190134814301));
#9396=CARTESIAN_POINT('Ctrl Pts',(-0.277520856446568,100.995821149692,6.05270722988584));
#9397=CARTESIAN_POINT('Ctrl Pts',(-0.219640398858692,100.995726175995,6.05332981198369));
#9398=CARTESIAN_POINT('Ctrl Pts',(-0.160514117704047,100.995663377514,6.05373046080009));
#9399=CARTESIAN_POINT('Ctrl Pts',(-0.0750025005669668,100.995572554963,
6.05430990072977));
#9400=CARTESIAN_POINT('Ctrl Pts',(0.0131158896791447,100.995550802574,6.05444281080532));
#9401=CARTESIAN_POINT('Ctrl Pts',(0.103931307124153,100.995613638244,6.05404463879305));
#9402=CARTESIAN_POINT('Ctrl Pts',(0.14533109622264,100.995642282978,6.05386312514926));
#9403=CARTESIAN_POINT('Ctrl Pts',(0.187291892296204,100.99568835001,6.05357083005548));
#9404=CARTESIAN_POINT('Ctrl Pts',(0.229824912171415,100.995752309851,6.053157457184));
#9405=CARTESIAN_POINT('Ctrl Pts',(0.311291713085964,100.995874817108,6.05236569197374));
#9406=CARTESIAN_POINT('Ctrl Pts',(0.394857584369436,100.996063677148,6.05112790481686));
#9407=CARTESIAN_POINT('Ctrl Pts',(0.480689955873217,100.996315037781,6.0493902677801));
#9408=CARTESIAN_POINT('Ctrl Pts',(0.537970868394036,100.996482785289,6.04823064194953));
#9409=CARTESIAN_POINT('Ctrl Pts',(0.59626182469888,100.996678124709,6.04684771747587));
#9410=CARTESIAN_POINT('Ctrl Pts',(0.655620049589673,100.996895635349,6.04521569132172));
#9411=CARTESIAN_POINT('Ctrl Pts',(0.743812153458893,100.997218804058,6.04279089138255));
#9412=CARTESIAN_POINT('Ctrl Pts',(0.834359954557442,100.997592544038,6.03982029829353));
#9413=CARTESIAN_POINT('Ctrl Pts',(0.927324292569222,100.997981133951,6.0362495538679));
#9414=CARTESIAN_POINT('Ctrl Pts',(0.990688253627786,100.998245994613,6.03381575489106));
#9415=CARTESIAN_POINT('Ctrl Pts',(1.05517562490491,100.998517286263,6.03110279618582));
#9416=CARTESIAN_POINT('Ctrl Pts',(1.12081525832687,100.998775489428,6.02808737922721));
#9417=CARTESIAN_POINT('Ctrl Pts',(1.20525737992653,100.999107654949,6.02420819538326));
#9418=CARTESIAN_POINT('Ctrl Pts',(1.29160708145152,100.999419290475,6.01982506746926));
#9419=CARTESIAN_POINT('Ctrl Pts',(1.37999323522187,100.999648545207,6.01491167471667));
#9420=CARTESIAN_POINT('Ctrl Pts',(1.46111364923389,100.999858954168,6.01040218496865));
#9421=CARTESIAN_POINT('Ctrl Pts',(1.54394986559642,101.,6.00544603395953));
#9422=CARTESIAN_POINT('Ctrl Pts',(1.628621697537,101.,5.999999999856));
#9423=CARTESIAN_POINT('Ctrl Pts',(-1.689481893123,102.1196847108,6.992808061201));
#9424=CARTESIAN_POINT('Ctrl Pts',(-1.669187233917,102.1197065598,6.992808061201));
#9425=CARTESIAN_POINT('Ctrl Pts',(-1.512636201126,102.1197869626,6.992808061201));
#9426=CARTESIAN_POINT('Ctrl Pts',(-1.23556503978,102.1188276871,6.992808061201));
#9427=CARTESIAN_POINT('Ctrl Pts',(-0.8648101546223,102.1166806136,6.992808061201));
#9428=CARTESIAN_POINT('Ctrl Pts',(-0.5109811635092,102.1148120947,6.992808061201));
#9429=CARTESIAN_POINT('Ctrl Pts',(-0.1488522802808,102.1137128273,6.992808061201));
#9430=CARTESIAN_POINT('Ctrl Pts',(0.2394130054686,102.1138378158,6.992808061201));
#9431=CARTESIAN_POINT('Ctrl Pts',(0.663639050088,102.1154833678,6.992808061201));
#9432=CARTESIAN_POINT('Ctrl Pts',(1.130096203131,102.1183003163,6.992808061201));
#9433=CARTESIAN_POINT('Ctrl Pts',(1.477116016106,102.1198046106,6.992808061201));
#9434=CARTESIAN_POINT('Ctrl Pts',(1.669209716084,102.1197066226,6.992808061201));
#9435=CARTESIAN_POINT('Ctrl Pts',(1.689515664192,102.1196849348,6.992808061201));
#9436=CARTESIAN_POINT('Ctrl Pts',(-1.688715228218,101.4207068678,7.077093790264));
#9437=CARTESIAN_POINT('Ctrl Pts',(-1.668689128932,101.4207284853,7.077093790264));
#9438=CARTESIAN_POINT('Ctrl Pts',(-1.514109227167,101.4208080916,7.077093790264));
#9439=CARTESIAN_POINT('Ctrl Pts',(-1.239188923109,101.4198586149,7.077093790264));
#9440=CARTESIAN_POINT('Ctrl Pts',(-0.8689370512758,101.41771466,7.077093790264));
#9441=CARTESIAN_POINT('Ctrl Pts',(-0.5140416525734,101.4158400361,7.077093790264));
#9442=CARTESIAN_POINT('Ctrl Pts',(-0.1498433242845,101.4147339759,7.077093790264));
#9443=CARTESIAN_POINT('Ctrl Pts',(0.2409905058727,101.4148598525,7.077093790264));
#9444=CARTESIAN_POINT('Ctrl Pts',(0.667428084141,101.4165149357,7.077093790264));
#9445=CARTESIAN_POINT('Ctrl Pts',(1.134325060388,101.4193353122,7.077093790264));
#9446=CARTESIAN_POINT('Ctrl Pts',(1.479036591025,101.4208256727,7.077093790264));
#9447=CARTESIAN_POINT('Ctrl Pts',(1.668711295896,101.4207285315,7.077093790264));
#9448=CARTESIAN_POINT('Ctrl Pts',(1.688748453112,101.4207070467,7.077093790264));
#9449=CARTESIAN_POINT('Ctrl Pts',(-1.68816918717,100.9228745154,6.579261201271));
#9450=CARTESIAN_POINT('Ctrl Pts',(-1.668334364073,100.922895968,6.579261201271));
#9451=CARTESIAN_POINT('Ctrl Pts',(-1.515158359163,100.9229750071,6.579261201271));
#9452=CARTESIAN_POINT('Ctrl Pts',(-1.241769958231,100.9220325094,6.579261201271));
#9453=CARTESIAN_POINT('Ctrl Pts',(-0.8718763471198,100.9198907756,6.579261201271));
#9454=CARTESIAN_POINT('Ctrl Pts',(-0.5162214219115,100.9180118035,6.579261201271));
#9455=CARTESIAN_POINT('Ctrl Pts',(-0.1505491746523,100.9169009054,6.579261201271));
#9456=CARTESIAN_POINT('Ctrl Pts',(0.2421140475483,100.9170274144,6.579261201271));
#9457=CARTESIAN_POINT('Ctrl Pts',(0.6701267444128,100.918689286,6.579261201271));
#9458=CARTESIAN_POINT('Ctrl Pts',(1.137336975539,100.9215121041,6.579261201271));
#9459=CARTESIAN_POINT('Ctrl Pts',(1.480404480349,100.9229925405,6.579261201271));
#9460=CARTESIAN_POINT('Ctrl Pts',(1.668356306539,100.9228960023,6.579261201271));
#9461=CARTESIAN_POINT('Ctrl Pts',(1.688202023064,100.9228746621,6.579261201271));
#9462=CARTESIAN_POINT('Ctrl Pts',(-1.688261634851,101.0071602049,5.880283026469));
#9463=CARTESIAN_POINT('Ctrl Pts',(-1.668394427668,101.0071816854,5.880283026469));
#9464=CARTESIAN_POINT('Ctrl Pts',(-1.514980735485,101.0072608205,5.880283026469));
#9465=CARTESIAN_POINT('Ctrl Pts',(-1.241332975131,101.0063171412,5.880283026469));
#9466=CARTESIAN_POINT('Ctrl Pts',(-0.8713787085563,101.0041750314,5.880283026469));
#9467=CARTESIAN_POINT('Ctrl Pts',(-0.5158523752623,101.0022967954,5.880283026469));
#9468=CARTESIAN_POINT('Ctrl Pts',(-0.1504296703963,101.0011867164,5.880283026469));
#9469=CARTESIAN_POINT('Ctrl Pts',(0.2419238259119,101.0013131184,5.880283026469));
#9470=CARTESIAN_POINT('Ctrl Pts',(0.6696698467433,101.0029738406,5.880283026469));
#9471=CARTESIAN_POINT('Ctrl Pts',(1.136827042137,101.0057962454,5.880283026469));
#9472=CARTESIAN_POINT('Ctrl Pts',(1.480172889344,101.007278362,5.880283026469));
#9473=CARTESIAN_POINT('Ctrl Pts',(1.668416408143,101.0071817217,5.880283026469));
#9474=CARTESIAN_POINT('Ctrl Pts',(1.688294536604,101.007160357,5.880283026469));
#9475=CARTESIAN_POINT('Origin',(-1.628604434127,102.,6.));
#9476=CARTESIAN_POINT('Origin',(1.628621700447,102.,6.));
#9477=CARTESIAN_POINT('Origin',(-8.153768,102.,6.));
#9478=CARTESIAN_POINT('Origin',(7.,102.,6.));
#9479=CARTESIAN_POINT('Origin',(7.,102.,6.));
#9480=CARTESIAN_POINT('Origin',(-75.7512,102.,6.));
#9481=CARTESIAN_POINT('Origin',(-7.,102.,6.));
#9482=CARTESIAN_POINT('Origin',(-7.,102.,6.));
#9483=CARTESIAN_POINT('',(-8.,102.,6.));
#9484=CARTESIAN_POINT('Origin',(-7.,102.,6.));
#9485=CARTESIAN_POINT('Origin',(-7.,102.,6.));
#9486=CARTESIAN_POINT('Origin',(-7.,102.,43.78380184031));
#9487=CARTESIAN_POINT('',(-8.,102.,-6.));
#9488=CARTESIAN_POINT('',(-8.,102.,6.));
#9489=CARTESIAN_POINT('Origin',(-7.,102.,-6.));
#9490=CARTESIAN_POINT('Origin',(-7.,102.,-6.));
#9491=CARTESIAN_POINT('Origin',(-7.,102.,-6.));
#9492=CARTESIAN_POINT('Origin',(-7.,-138.3504337905,-6.));
#9493=CARTESIAN_POINT('',(-8.,116.,-6.));
#9494=CARTESIAN_POINT('',(-8.,102.,-6.));
#9495=CARTESIAN_POINT('Origin',(-7.,116.,-6.));
#9496=CARTESIAN_POINT('Origin',(-8.,117.,-7.));
#9497=CARTESIAN_POINT('',(-8.,116.,6.));
#9498=CARTESIAN_POINT('',(-8.,116.,6.));
#9499=CARTESIAN_POINT('',(-8.,116.,6.));
#9500=CARTESIAN_POINT('Origin',(-7.,116.,43.78380184031));
#9501=CARTESIAN_POINT('',(-7.,117.,6.));
#9502=CARTESIAN_POINT('Origin',(-7.,116.,6.));
#9503=CARTESIAN_POINT('',(-7.,117.,-6.));
#9504=CARTESIAN_POINT('',(-7.,117.,6.));
#9505=CARTESIAN_POINT('Origin',(-7.,116.,-6.));
#9506=CARTESIAN_POINT('Origin',(-7.,116.,-6.));
#9507=CARTESIAN_POINT('Origin',(-7.,116.,-6.));
#9508=CARTESIAN_POINT('Origin',(-75.7512,116.,-6.));
#9509=CARTESIAN_POINT('',(7.,117.,-6.));
#9510=CARTESIAN_POINT('',(-7.,117.,-6.));
#9511=CARTESIAN_POINT('Origin',(7.,116.,-6.));
#9512=CARTESIAN_POINT('Origin',(7.,116.,-6.));
#9513=CARTESIAN_POINT('Origin',(7.,116.,-6.));
#9514=CARTESIAN_POINT('Origin',(7.,116.,-6.));
#9515=CARTESIAN_POINT('Origin',(7.,269.5212,-6.));
#9516=CARTESIAN_POINT('Origin',(7.,116.,43.78380184031));
#9517=CARTESIAN_POINT('',(7.,117.,6.));
#9518=CARTESIAN_POINT('',(7.,117.,6.));
#9519=CARTESIAN_POINT('Origin',(7.,116.,6.));
#9520=CARTESIAN_POINT('Origin',(8.,117.,-7.));
#9521=CARTESIAN_POINT('',(7.,117.,6.));
#9522=CARTESIAN_POINT('',(-4.,117.,4.89858719658941E-16));
#9523=CARTESIAN_POINT('Origin',(0.,117.,0.));
#9524=CARTESIAN_POINT('Origin',(75.7512,116.,6.));
#9525=CARTESIAN_POINT('Origin',(-7.,116.,6.));
#9526=CARTESIAN_POINT('Origin',(7.,116.,6.));
#9527=CARTESIAN_POINT('Origin',(7.,116.,6.));
#9528=CARTESIAN_POINT('Origin',(-7.,116.,6.));
#9529=CARTESIAN_POINT('Origin',(-7.,116.,6.));
#9530=CARTESIAN_POINT('Origin',(-7.,269.5212,6.));
#9531=CARTESIAN_POINT('Origin',(0.,117.,0.));
#9532=CARTESIAN_POINT('',(-4.,120.,4.89858719658941E-16));
#9533=CARTESIAN_POINT('Origin',(0.,120.,0.));
#9534=CARTESIAN_POINT('',(-4.,117.,4.89858719658941E-16));
#9535=CARTESIAN_POINT('Origin',(0.,120.,-7.));
#9536=CARTESIAN_POINT('',(-1.5,120.,1.83697019872103E-16));
#9537=CARTESIAN_POINT('Origin',(0.,120.,0.));
#9538=CARTESIAN_POINT('Origin',(0.,119.875,0.));
#9539=CARTESIAN_POINT('',(-1.25,119.75,1.5308084989342E-16));
#9540=CARTESIAN_POINT('Origin',(0.,119.75,0.));
#9541=CARTESIAN_POINT('',(-1.375,119.875,1.68388934882761E-16));
#9542=CARTESIAN_POINT('Origin',(0.,109.7613704375,0.));
#9543=CARTESIAN_POINT('',(-1.25,109.7613704375,1.53080849893419E-16));
#9544=CARTESIAN_POINT('Origin',(0.,69.72097410502,0.));
#9545=CARTESIAN_POINT('',(0.,47.91425627512,6.712116818331));
#9546=CARTESIAN_POINT('',(6.71211681833062,47.91425627512,8.21997237707171E-16));
#9547=CARTESIAN_POINT('Origin',(0.,47.91425627512,0.));
#9548=CARTESIAN_POINT('',(5.187242561534,69.72097410502,6.35253999938353E-16));
#9549=CARTESIAN_POINT('Origin',(0.,47.91425627512,0.));
#9550=CARTESIAN_POINT('Origin',(0.,69.72097410502,0.));
#9551=CARTESIAN_POINT('',(7.15007114377336,41.65121763128,8.75631173989789E-16));
#9552=CARTESIAN_POINT('',(0.0106247171632265,41.65121763128,7.15006324981918));
#9553=CARTESIAN_POINT('Origin',(0.,41.65121763128,0.));
#9554=CARTESIAN_POINT('Origin',(0.,41.65121763128,0.));
#9555=CARTESIAN_POINT('',(7.11077262920686,42.2132125724799,8.70818493982279E-16));
#9556=CARTESIAN_POINT('',(5.187242561534,69.72097410502,6.35253999938353E-16));
#9557=CARTESIAN_POINT('',(0.,42.21321257248,7.110772629208));
#9558=CARTESIAN_POINT('Origin',(0.,42.21321257248,0.));
#9559=CARTESIAN_POINT('Origin',(0.,42.21321257248,0.));
#9560=CARTESIAN_POINT('Origin',(0.,45.,0.));
#9561=CARTESIAN_POINT('Origin',(7.34788079488412E-16,45.,6.));
#9562=CARTESIAN_POINT('Origin',(0.,42.,0.));
#9563=CARTESIAN_POINT('',(0.011887692143076,39.1932353328207,8.00000000000279));
#9564=CARTESIAN_POINT('Origin',(0.0180364167624925,42.,12.1378779943689));
#9565=CARTESIAN_POINT('',(9.1284394897767,37.,8.));
#9566=CARTESIAN_POINT('Ctrl Pts',(9.12843948977668,37.,8.));
#9567=CARTESIAN_POINT('Ctrl Pts',(8.57403140594617,37.,8.));
#9568=CARTESIAN_POINT('Ctrl Pts',(7.96896895550773,37.0558564477204,8.));
#9569=CARTESIAN_POINT('Ctrl Pts',(6.77413711943837,37.2666014130387,8.));
#9570=CARTESIAN_POINT('Ctrl Pts',(6.18411009233275,37.4200265971388,8.));
#9571=CARTESIAN_POINT('Ctrl Pts',(4.75709729947724,37.8565700407443,8.));
#9572=CARTESIAN_POINT('Ctrl Pts',(3.80441040251253,38.2365947939282,8.));
#9573=CARTESIAN_POINT('Ctrl Pts',(1.90336768275116,38.9163280810235,8.));
#9574=CARTESIAN_POINT('Ctrl Pts',(0.946007958016012,39.1911889725053,8.));
#9575=CARTESIAN_POINT('Ctrl Pts',(0.0118876940187937,39.1932353328207,8.));
#9576=CARTESIAN_POINT('',(11.0000000430061,36.9999999999999,5.13112121888498));
#9577=CARTESIAN_POINT('Origin',(0.,37.,0.));
#9578=CARTESIAN_POINT('',(11.1896485656096,37.0907398175677,-0.000169479335991176));
#9579=CARTESIAN_POINT('Ctrl Pts',(11.0000000164978,36.9999999999997,5.13112121714035));
#9580=CARTESIAN_POINT('Ctrl Pts',(11.0111825439989,36.9999999953411,4.96121154043948));
#9581=CARTESIAN_POINT('Ctrl Pts',(11.0218701867737,37.0011359668517,4.79400389659548));
#9582=CARTESIAN_POINT('Ctrl Pts',(11.0320046124329,37.0030129927172,4.63027386211126));
#9583=CARTESIAN_POINT('Ctrl Pts',(11.0387890381477,37.0042695555436,4.52066584942374));
#9584=CARTESIAN_POINT('Ctrl Pts',(11.0453260204498,37.0058588915485,4.41261648872546));
#9585=CARTESIAN_POINT('Ctrl Pts',(11.0516043222841,37.0076742438597,4.30635962787506));
#9586=CARTESIAN_POINT('Ctrl Pts',(11.0588074658838,37.0097570114179,4.18445032065147));
#9587=CARTESIAN_POINT('Ctrl Pts',(11.065661238494,37.0121352203763,4.06489359579171));
#9588=CARTESIAN_POINT('Ctrl Pts',(11.072247928066,37.0147222240793,3.94622081445611));
#9589=CARTESIAN_POINT('Ctrl Pts',(11.0795239743893,37.0175799811627,3.81512785115984));
#9590=CARTESIAN_POINT('Ctrl Pts',(11.0864749761023,37.0206940009696,3.68511373779337));
#9591=CARTESIAN_POINT('Ctrl Pts',(11.0931851556689,37.0239939869192,3.55417020202618));
#9592=CARTESIAN_POINT('Ctrl Pts',(11.0936038808397,37.0241999109435,3.54599913091845));
#9593=CARTESIAN_POINT('Ctrl Pts',(11.0940216577092,37.024406568043,3.53782443170898));
#9594=CARTESIAN_POINT('Ctrl Pts',(11.0944385023882,37.0246139441538,3.52964561286928));
#9595=CARTESIAN_POINT('Ctrl Pts',(11.1035557560452,37.0291496878003,3.35075796061484));
#9596=CARTESIAN_POINT('Ctrl Pts',(11.1122444065986,37.0340295031561,3.16991671730982));
#9597=CARTESIAN_POINT('Ctrl Pts',(11.1204316981979,37.0390274579943,2.98613137636941));
#9598=CARTESIAN_POINT('Ctrl Pts',(11.1240477545458,37.0412348896096,2.90495946002643));
#9599=CARTESIAN_POINT('Ctrl Pts',(11.1275655528008,37.0434650373592,2.82321306518882));
#9600=CARTESIAN_POINT('Ctrl Pts',(11.1309764107165,37.0456961209886,2.74080610561445));
#9601=CARTESIAN_POINT('Ctrl Pts',(11.1376689356853,37.0500737829335,2.57911346165467));
#9602=CARTESIAN_POINT('Ctrl Pts',(11.1439502033684,37.05445742758,2.41487893318168));
#9603=CARTESIAN_POINT('Ctrl Pts',(11.1497597449324,37.0586941757249,2.24739586736983));
#9604=CARTESIAN_POINT('Ctrl Pts',(11.1536148395963,37.0615055963827,2.1362574812872));
#9605=CARTESIAN_POINT('Ctrl Pts',(11.1572616759657,37.0642517494188,2.02368854786336));
#9606=CARTESIAN_POINT('Ctrl Pts',(11.1606749001187,37.0668775563969,1.90948220592755));
#9607=CARTESIAN_POINT('Ctrl Pts',(11.1649533384812,37.0701689761234,1.76632583157622));
#9608=CARTESIAN_POINT('Ctrl Pts',(11.1688593820582,37.0732744443208,1.62059725365725));
#9609=CARTESIAN_POINT('Ctrl Pts',(11.1723451311472,37.0761105840506,1.47105010106573));
#9610=CARTESIAN_POINT('Ctrl Pts',(11.1755030580699,37.0786799950381,1.33556732037411));
#9611=CARTESIAN_POINT('Ctrl Pts',(11.1783159006795,37.0810286574292,1.19695011526774));
#9612=CARTESIAN_POINT('Ctrl Pts',(11.1807164562182,37.0830600739771,1.05427204426782));
#9613=CARTESIAN_POINT('Ctrl Pts',(11.1809656561954,37.083270953896,1.03946073435624));
#9614=CARTESIAN_POINT('Ctrl Pts',(11.1812103833398,37.0834783790926,1.02460566578708));
#9615=CARTESIAN_POINT('Ctrl Pts',(11.1814505411601,37.0836822154566,1.00970580448101));
#9616=CARTESIAN_POINT('Ctrl Pts',(11.1844070041638,37.086191543149,0.826281052145604));
#9617=CARTESIAN_POINT('Ctrl Pts',(11.1866861367669,37.0881564592366,0.636073731167722));
#9618=CARTESIAN_POINT('Ctrl Pts',(11.1880832646347,37.0893710087782,0.439358371355146));
#9619=CARTESIAN_POINT('Ctrl Pts',(11.1890996419792,37.0902545647264,0.296252618727001));
#9620=CARTESIAN_POINT('Ctrl Pts',(11.1896489896218,37.0907404613239,0.149703434419743));
#9621=CARTESIAN_POINT('Ctrl Pts',(11.1896485656097,37.0907398175686,-0.000169479335990849));
#9622=CARTESIAN_POINT('',(11.00000001131,36.9999999999996,-5.1311213989913));
#9623=CARTESIAN_POINT('Ctrl Pts',(11.1896485656095,37.0907398175672,-0.000169481921701897));
#9624=CARTESIAN_POINT('Ctrl Pts',(11.1896479776106,37.0907393489086,-0.215681937420152));
#9625=CARTESIAN_POINT('Ctrl Pts',(11.1885084096789,37.0897437526926,-0.429458199024161));
#9626=CARTESIAN_POINT('Ctrl Pts',(11.1863420983071,37.0878649344339,-0.640356926161641));
#9627=CARTESIAN_POINT('Ctrl Pts',(11.1848579333,37.0865777342879,-0.784846086366657));
#9628=CARTESIAN_POINT('Ctrl Pts',(11.1828937972378,37.0848807618758,-0.927983658842167));
#9629=CARTESIAN_POINT('Ctrl Pts',(11.1804313296578,37.0828103697687,-1.07149129532294));
#9630=CARTESIAN_POINT('Ctrl Pts',(11.1792995395267,37.0818587838987,-1.1374497379955));
#9631=CARTESIAN_POINT('Ctrl Pts',(11.1780624885594,37.0808275508911,-1.20348625455482));
#9632=CARTESIAN_POINT('Ctrl Pts',(11.1767184554982,37.079716688106,-1.26976720008837));
#9633=CARTESIAN_POINT('Ctrl Pts',(11.1737179373486,37.0772367164114,-1.41773765244469));
#9634=CARTESIAN_POINT('Ctrl Pts',(11.170180947628,37.0743547381601,-1.56692968835248));
#9635=CARTESIAN_POINT('Ctrl Pts',(11.1661975793124,37.0711980429517,-1.71481587196975));
#9636=CARTESIAN_POINT('Ctrl Pts',(11.1645145444965,37.0698642903287,-1.77730007531386));
#9637=CARTESIAN_POINT('Ctrl Pts',(11.162751830014,37.068482172809,-1.83955138112467));
#9638=CARTESIAN_POINT('Ctrl Pts',(11.1609162604204,37.0670636502293,-1.90138036125891));
#9639=CARTESIAN_POINT('Ctrl Pts',(11.1556956020255,37.0630291413554,-2.07723203439244));
#9640=CARTESIAN_POINT('Ctrl Pts',(11.1498881311807,37.05870533442,-2.24966268054424));
#9641=CARTESIAN_POINT('Ctrl Pts',(11.1435805979118,37.0542623608385,-2.41970231738112));
#9642=CARTESIAN_POINT('Ctrl Pts',(11.1424215894495,37.0534459649894,-2.45094707973465));
#9643=CARTESIAN_POINT('Ctrl Pts',(11.1412457008067,37.0526254051766,-2.48211109005339));
#9644=CARTESIAN_POINT('Ctrl Pts',(11.1400534753533,37.0518015675164,-2.51320070664233));
#9645=CARTESIAN_POINT('Ctrl Pts',(11.1340795973032,37.0476735683188,-2.66898129125717));
#9646=CARTESIAN_POINT('Ctrl Pts',(11.1276955664116,37.0434656559455,-2.82289198400398));
#9647=CARTESIAN_POINT('Ctrl Pts',(11.1207794793186,37.0392364138983,-2.97845296202742));
#9648=CARTESIAN_POINT('Ctrl Pts',(11.118803649819,37.0380281785066,-3.02289456104516));
#9649=CARTESIAN_POINT('Ctrl Pts',(11.1167844246291,37.0368181061012,-3.06747053813211));
#9650=CARTESIAN_POINT('Ctrl Pts',(11.1147190384397,37.0356076179028,-3.11226217733893));
#9651=CARTESIAN_POINT('Ctrl Pts',(11.1083673846949,37.0318850201926,-3.25000928941724));
#9652=CARTESIAN_POINT('Ctrl Pts',(11.101578293801,37.0281556654332,-3.3897989420054));
#9653=CARTESIAN_POINT('Ctrl Pts',(11.0942772760587,37.0245331428097,-3.53281226756565));
#9654=CARTESIAN_POINT('Ctrl Pts',(11.0908940504137,37.0228544985615,-3.59908335026864));
#9655=CARTESIAN_POINT('Ctrl Pts',(11.0874009596442,37.0211993154306,-3.66604635730229));
#9656=CARTESIAN_POINT('Ctrl Pts',(11.0837909632952,37.0195825443791,-3.73381714784607));
#9657=CARTESIAN_POINT('Ctrl Pts',(11.0771004661201,37.0165861418603,-3.85941846121413));
#9658=CARTESIAN_POINT('Ctrl Pts',(11.0700080901534,37.0137189253489,-3.98779522803996));
#9659=CARTESIAN_POINT('Ctrl Pts',(11.0624744656947,37.0111220264858,-4.11941195521222));
#9660=CARTESIAN_POINT('Ctrl Pts',(11.0571710426893,37.0092938953851,-4.21206578772226));
#9661=CARTESIAN_POINT('Ctrl Pts',(11.0516490173313,37.0076004516683,-4.30632503899295));
#9662=CARTESIAN_POINT('Ctrl Pts',(11.0458959603966,37.0061063072661,-4.40234852950457));
#9663=CARTESIAN_POINT('Ctrl Pts',(11.0383442029163,37.0041450167219,-4.52839388608507));
#9664=CARTESIAN_POINT('Ctrl Pts',(11.0303942662333,37.0025253678984,-4.65747976771746));
#9665=CARTESIAN_POINT('Ctrl Pts',(11.0220365153567,37.0014432233025,-4.78968265020428));
#9666=CARTESIAN_POINT('Ctrl Pts',(11.0149826233968,37.0005298997089,-4.90126109560603));
#9667=CARTESIAN_POINT('Ctrl Pts',(11.0076382775635,36.9999999853001,-5.01505974973993));
#9668=CARTESIAN_POINT('Ctrl Pts',(11.000000004389,36.9999999999982,-5.13112139853582));
#9669=CARTESIAN_POINT('',(9.12843948977674,36.9999999999999,-8.00000000000001));
#9670=CARTESIAN_POINT('Origin',(0.,37.,0.));
#9671=CARTESIAN_POINT('',(-9.12843948977662,37.,-8.00000000000001));
#9672=CARTESIAN_POINT('Ctrl Pts',(-9.12843948977668,37.,-8.));
#9673=CARTESIAN_POINT('Ctrl Pts',(-8.57403140594617,37.,-8.));
#9674=CARTESIAN_POINT('Ctrl Pts',(-7.96896895550773,37.0558564477204,-8.));
#9675=CARTESIAN_POINT('Ctrl Pts',(-6.77413711943837,37.2666014130387,-8.));
#9676=CARTESIAN_POINT('Ctrl Pts',(-6.18411009233275,37.4200265971388,-8.));
#9677=CARTESIAN_POINT('Ctrl Pts',(-4.75709729947724,37.8565700407443,-8.));
#9678=CARTESIAN_POINT('Ctrl Pts',(-3.80441040251253,38.2365947939282,-8.));
#9679=CARTESIAN_POINT('Ctrl Pts',(-1.89934365236072,38.9177669058201,-8.));
#9680=CARTESIAN_POINT('Ctrl Pts',(-0.937884008599215,39.1932483539498,-8.));
#9681=CARTESIAN_POINT('Ctrl Pts',(0.,39.1932483539498,-8.));
#9682=CARTESIAN_POINT('Ctrl Pts',(0.937884008599215,39.1932483539498,-8.));
#9683=CARTESIAN_POINT('Ctrl Pts',(1.89934365236072,38.9177669058201,-8.));
#9684=CARTESIAN_POINT('Ctrl Pts',(3.80441040251253,38.2365947939282,-8.));
#9685=CARTESIAN_POINT('Ctrl Pts',(4.75709729947724,37.8565700407443,-8.));
#9686=CARTESIAN_POINT('Ctrl Pts',(6.18411009233275,37.4200265971388,-8.));
#9687=CARTESIAN_POINT('Ctrl Pts',(6.77413711943837,37.2666014130387,-8.));
#9688=CARTESIAN_POINT('Ctrl Pts',(7.96896895550773,37.0558564477204,-8.));
#9689=CARTESIAN_POINT('Ctrl Pts',(8.57403140594617,37.,-8.));
#9690=CARTESIAN_POINT('Ctrl Pts',(9.12843948977668,37.,-8.));
#9691=CARTESIAN_POINT('',(-11.0000003498417,36.9999999999996,-5.13111944275097));
#9692=CARTESIAN_POINT('Origin',(0.,37.,0.));
#9693=CARTESIAN_POINT('',(-11.0000000676958,36.9999999999997,5.1311211208313));
#9694=CARTESIAN_POINT('Ctrl Pts',(-11.00000002783,36.9999999999987,5.131121044419));
#9695=CARTESIAN_POINT('Ctrl Pts',(-11.0140712521959,36.9999998982868,4.91732288718392));
#9696=CARTESIAN_POINT('Ctrl Pts',(-11.0276242001948,37.0017973389252,4.70395369933127));
#9697=CARTESIAN_POINT('Ctrl Pts',(-11.0405748924402,37.0047974379781,4.49058332358683));
#9698=CARTESIAN_POINT('Ctrl Pts',(-11.0469128280474,37.0062656556033,4.38616205587838));
#9699=CARTESIAN_POINT('Ctrl Pts',(-11.0531064872421,37.0080228023865,4.28174026543605));
#9700=CARTESIAN_POINT('Ctrl Pts',(-11.0591455982534,37.0100032565513,4.17726625883438));
#9701=CARTESIAN_POINT('Ctrl Pts',(-11.0775247948997,37.0160304940826,3.85931411187551));
#9702=CARTESIAN_POINT('Ctrl Pts',(-11.0944748101117,37.0241218487547,3.54088391180374));
#9703=CARTESIAN_POINT('Ctrl Pts',(-11.1095943066205,37.0326593422877,3.22184910859468));
#9704=CARTESIAN_POINT('Ctrl Pts',(-11.1187140108614,37.0378089460416,3.02941525035502));
#9705=CARTESIAN_POINT('Ctrl Pts',(-11.1271734995192,37.0431206795202,2.8367637002585));
#9706=CARTESIAN_POINT('Ctrl Pts',(-11.134861631142,37.0482731329454,2.64520456823093));
#9707=CARTESIAN_POINT('Ctrl Pts',(-11.1399196013838,37.051662897504,2.51917909977126));
#9708=CARTESIAN_POINT('Ctrl Pts',(-11.1446444463466,37.0549837079099,2.39362690391072));
#9709=CARTESIAN_POINT('Ctrl Pts',(-11.1490146449952,37.0581507000346,2.26892480975772));
#9710=CARTESIAN_POINT('Ctrl Pts',(-11.1549415540522,37.0624458078356,2.0998025270654));
#9711=CARTESIAN_POINT('Ctrl Pts',(-11.1602029823346,37.066463069481,1.93223807087765));
#9712=CARTESIAN_POINT('Ctrl Pts',(-11.1648420582513,37.0701137654189,1.76477567623669));
#9713=CARTESIAN_POINT('Ctrl Pts',(-11.1688229474782,37.0732465048677,1.62107265117187));
#9714=CARTESIAN_POINT('Ctrl Pts',(-11.1723450969853,37.0761098710538,1.47744412273924));
#9715=CARTESIAN_POINT('Ctrl Pts',(-11.1754100328185,37.0786343854209,1.33295994640686));
#9716=CARTESIAN_POINT('Ctrl Pts',(-11.1787283416866,37.081367597099,1.17653150883889));
#9717=CARTESIAN_POINT('Ctrl Pts',(-11.1815094557598,37.0837049268536,1.01910414823258));
#9718=CARTESIAN_POINT('Ctrl Pts',(-11.1837157609282,37.0855863364246,0.859408825005803));
#9719=CARTESIAN_POINT('Ctrl Pts',(-11.1857777329768,37.0873446670504,0.710160526304185));
#9720=CARTESIAN_POINT('Ctrl Pts',(-11.1873375402417,37.0887050572166,0.558930819716984));
#9721=CARTESIAN_POINT('Ctrl Pts',(-11.1883298687427,37.0895851698554,0.40468523977506));
#9722=CARTESIAN_POINT('Ctrl Pts',(-11.1883993293682,37.0896467756385,0.393888417495881));
#9723=CARTESIAN_POINT('Ctrl Pts',(-11.188465994842,37.0897060127454,0.383076820735572));
#9724=CARTESIAN_POINT('Ctrl Pts',(-11.1885298360109,37.089762845708,0.372250095909413));
#9725=CARTESIAN_POINT('Ctrl Pts',(-11.1893515624725,37.0904943666063,0.232894779729622));
#9726=CARTESIAN_POINT('Ctrl Pts',(-11.1897251319801,37.0908203025814,0.091033038055436));
#9727=CARTESIAN_POINT('Ctrl Pts',(-11.1896061673193,37.0907133376148,-0.051869431910791));
#9728=CARTESIAN_POINT('Ctrl Pts',(-11.1894871572608,37.0906063318296,-0.194826434508157));
#9729=CARTESIAN_POINT('Ctrl Pts',(-11.1888751656669,37.0900661047587,-0.338824405220953));
#9730=CARTESIAN_POINT('Ctrl Pts',(-11.187764938011,37.0890997865693,-0.482392709589935));
#9731=CARTESIAN_POINT('Ctrl Pts',(-11.1873489450846,37.0887377153046,-0.53618654075308));
#9732=CARTESIAN_POINT('Ctrl Pts',(-11.1868634011007,37.0883161682624,-0.589920059916406));
#9733=CARTESIAN_POINT('Ctrl Pts',(-11.1863094553398,37.0878367426741,-0.64351603627636));
#9734=CARTESIAN_POINT('Ctrl Pts',(-11.184708991504,37.0864515830243,-0.798365893382707));
#9735=CARTESIAN_POINT('Ctrl Pts',(-11.1825307099028,37.0845819711465,-0.952073832901876));
#9736=CARTESIAN_POINT('Ctrl Pts',(-11.1798663337782,37.0823448383766,-1.10299844583809));
#9737=CARTESIAN_POINT('Ctrl Pts',(-11.1770641026185,37.079991956177,-1.26173191039888));
#9738=CARTESIAN_POINT('Ctrl Pts',(-11.1737243966345,37.0772335467755,-1.41738578506559));
#9739=CARTESIAN_POINT('Ctrl Pts',(-11.1700003378975,37.0742288059789,-1.56807286505966));
#9740=CARTESIAN_POINT('Ctrl Pts',(-11.1694993295277,37.0738245695277,-1.58834523282626));
#9741=CARTESIAN_POINT('Ctrl Pts',(-11.1689914265003,37.0734158935885,-1.60852774786708));
#9742=CARTESIAN_POINT('Ctrl Pts',(-11.1684770570016,37.0730031797098,-1.6286158554092));
#9743=CARTESIAN_POINT('Ctrl Pts',(-11.1647599161538,37.0700206630152,-1.77378450421377));
#9744=CARTESIAN_POINT('Ctrl Pts',(-11.160686642056,37.0668348340176,-1.91401538308741));
#9745=CARTESIAN_POINT('Ctrl Pts',(-11.1563544893698,37.0635682346049,-2.04984526937032));
#9746=CARTESIAN_POINT('Ctrl Pts',(-11.1516936488259,37.0600537926897,-2.19598080219131));
#9747=CARTESIAN_POINT('Ctrl Pts',(-11.1467331069504,37.0564454021741,-2.33702237230987));
#9748=CARTESIAN_POINT('Ctrl Pts',(-11.1415612051114,37.0528467225342,-2.47364127210357));
#9749=CARTESIAN_POINT('Ctrl Pts',(-11.1412292039677,37.052615711623,-2.4824112821301));
#9750=CARTESIAN_POINT('Ctrl Pts',(-11.1408963216095,37.0523847266039,-2.49116306766433));
#9751=CARTESIAN_POINT('Ctrl Pts',(-11.1405625772943,37.0521537893321,-2.49989680636301));
#9752=CARTESIAN_POINT('Ctrl Pts',(-11.134890548819,37.0482289800629,-2.64832784276284));
#9753=CARTESIAN_POINT('Ctrl Pts',(-11.1289763642823,37.044321766251,-2.79154494313647));
#9754=CARTESIAN_POINT('Ctrl Pts',(-11.1229071577116,37.0405521348536,-2.9300690866496));
#9755=CARTESIAN_POINT('Ctrl Pts',(-11.1178853359213,37.0374330422883,-3.04468762109334));
#9756=CARTESIAN_POINT('Ctrl Pts',(-11.1127566977551,37.0344068277067,-3.15609321605914));
#9757=CARTESIAN_POINT('Ctrl Pts',(-11.1075567552947,37.0315187150892,-3.26458007893159));
#9758=CARTESIAN_POINT('Ctrl Pts',(-11.1004464312207,37.0275695527995,-3.41292340362817));
#9759=CARTESIAN_POINT('Ctrl Pts',(-11.0932054709357,37.0238800107333,-3.55580866728893));
#9760=CARTESIAN_POINT('Ctrl Pts',(-11.0859024624725,37.0205377067675,-3.69402073450888));
#9761=CARTESIAN_POINT('Ctrl Pts',(-11.0814098321309,37.0184816039595,-3.7790453828982));
#9762=CARTESIAN_POINT('Ctrl Pts',(-11.0768930183602,37.0165558606314,-3.86230134249087));
#9763=CARTESIAN_POINT('Ctrl Pts',(-11.0723622744047,37.0147735012423,-3.94396971338329));
#9764=CARTESIAN_POINT('Ctrl Pts',(-11.0638397053627,37.0114207889504,-4.0975922390254));
#9765=CARTESIAN_POINT('Ctrl Pts',(-11.055271239492,37.008575969418,-4.24559707805008));
#9766=CARTESIAN_POINT('Ctrl Pts',(-11.0466513754209,37.0063032181303,-4.38975182817902));
#9767=CARTESIAN_POINT('Ctrl Pts',(-11.0432397280449,37.0054036881721,-4.44680669249741));
#9768=CARTESIAN_POINT('Ctrl Pts',(-11.0398195142528,37.004593589514,-4.50325814803838));
#9769=CARTESIAN_POINT('Ctrl Pts',(-11.0363885793265,37.0038767568708,-4.5592146232255));
#9770=CARTESIAN_POINT('Ctrl Pts',(-11.0281541333304,37.0021563162868,-4.69351346099501));
#9771=CARTESIAN_POINT('Ctrl Pts',(-11.0198635189573,37.0009770903936,-4.82496577179628));
#9772=CARTESIAN_POINT('Ctrl Pts',(-11.0116031991166,37.0004045381099,-4.95304618956424));
#9773=CARTESIAN_POINT('Ctrl Pts',(-11.0077259733317,37.0001357937368,-5.01316452733983));
#9774=CARTESIAN_POINT('Ctrl Pts',(-11.0038553876797,36.9999999968381,-5.0725401265193));
#9775=CARTESIAN_POINT('Ctrl Pts',(-11.0000001341984,36.9999999999985,-5.13111942855892));
#9776=CARTESIAN_POINT('',(-9.12843948977677,37.,8.00000000000001));
#9777=CARTESIAN_POINT('Origin',(0.,37.,0.));
#9778=CARTESIAN_POINT('Ctrl Pts',(0.0118876940187937,39.1932353328207,8.));
#9779=CARTESIAN_POINT('Ctrl Pts',(0.00792470899211094,39.1932440144601,
8.));
#9780=CARTESIAN_POINT('Ctrl Pts',(0.00396214332439191,39.1932483539498,
8.));
#9781=CARTESIAN_POINT('Ctrl Pts',(0.,39.1932483539498,8.));
#9782=CARTESIAN_POINT('Ctrl Pts',(-0.937884008599215,39.1932483539498,8.));
#9783=CARTESIAN_POINT('Ctrl Pts',(-1.89934365236072,38.9177669058201,8.));
#9784=CARTESIAN_POINT('Ctrl Pts',(-3.80441040251253,38.2365947939282,8.));
#9785=CARTESIAN_POINT('Ctrl Pts',(-4.75709729947724,37.8565700407443,8.));
#9786=CARTESIAN_POINT('Ctrl Pts',(-6.18411009233275,37.4200265971388,8.));
#9787=CARTESIAN_POINT('Ctrl Pts',(-6.77413711943837,37.2666014130387,8.));
#9788=CARTESIAN_POINT('Ctrl Pts',(-7.96896895550773,37.0558564477204,8.));
#9789=CARTESIAN_POINT('Ctrl Pts',(-8.57403140594617,37.,8.));
#9790=CARTESIAN_POINT('Ctrl Pts',(-9.12843948977668,37.,8.));
#9791=CARTESIAN_POINT('Ctrl Pts',(-11.99357518999,35.88698149802,5.234127330856));
#9792=CARTESIAN_POINT('Ctrl Pts',(-11.99332528583,35.88468341677,5.199787902682));
#9793=CARTESIAN_POINT('Ctrl Pts',(-11.9906318297,35.86116870728,4.838104020626));
#9794=CARTESIAN_POINT('Ctrl Pts',(-11.98427746894,35.82995506373,4.152393802744));
#9795=CARTESIAN_POINT('Ctrl Pts',(-11.97368392242,35.80923437147,3.185041719748));
#9796=CARTESIAN_POINT('Ctrl Pts',(-11.96358545097,35.80256970675,2.237007562812));
#9797=CARTESIAN_POINT('Ctrl Pts',(-11.95575094264,35.80219571054,1.29827724728));
#9798=CARTESIAN_POINT('Ctrl Pts',(-11.95157858187,35.80318886163,0.346223922685));
#9799=CARTESIAN_POINT('Ctrl Pts',(-11.9522728448,35.80297211912,-0.619776846157));
#9800=CARTESIAN_POINT('Ctrl Pts',(-11.95764819515,35.80198588038,-1.560160325752));
#9801=CARTESIAN_POINT('Ctrl Pts',(-11.96556360283,35.80346825475,-2.425528994248));
#9802=CARTESIAN_POINT('Ctrl Pts',(-11.97385262721,35.81036052627,-3.197996220919));
#9803=CARTESIAN_POINT('Ctrl Pts',(-11.98141321701,35.82435952006,-3.892356813202));
#9804=CARTESIAN_POINT('Ctrl Pts',(-11.98781352018,35.84649412881,-4.527903781733));
#9805=CARTESIAN_POINT('Ctrl Pts',(-11.9916054427,35.86966712868,-4.968832637213));
#9806=CARTESIAN_POINT('Ctrl Pts',(-11.99332547808,35.88468592982,-5.199824834647));
#9807=CARTESIAN_POINT('Ctrl Pts',(-11.99357531375,35.88698559565,-5.234182558824));
#9808=CARTESIAN_POINT('Ctrl Pts',(-12.07325730637,36.58649630964,5.231935522022));
#9809=CARTESIAN_POINT('Ctrl Pts',(-12.07454985414,36.58402482358,5.198345177035));
#9810=CARTESIAN_POINT('Ctrl Pts',(-12.08802346863,36.55862535039,4.844356710033));
#9811=CARTESIAN_POINT('Ctrl Pts',(-12.11067089349,36.52274336209,4.169388296033));
#9812=CARTESIAN_POINT('Ctrl Pts',(-12.13520968347,36.49435585584,3.208216487448));
#9813=CARTESIAN_POINT('Ctrl Pts',(-12.15233416592,36.48062816741,2.258775260772));
#9814=CARTESIAN_POINT('Ctrl Pts',(-12.16302208196,36.4749403482,1.313089996961));
#9815=CARTESIAN_POINT('Ctrl Pts',(-12.16800326631,36.47316053362,0.3504770567543));
#9816=CARTESIAN_POINT('Ctrl Pts',(-12.1672071462,36.47340225696,-0.6273013998855));
#9817=CARTESIAN_POINT('Ctrl Pts',(-12.16060767632,36.47600423761,-1.577345655872));
#9818=CARTESIAN_POINT('Ctrl Pts',(-12.1491868573,36.48289948249,-2.447846195142));
#9819=CARTESIAN_POINT('Ctrl Pts',(-12.13442993541,36.49562105325,-3.220605537441));
#9820=CARTESIAN_POINT('Ctrl Pts',(-12.117320878,36.51507009099,-3.911064023649));
#9821=CARTESIAN_POINT('Ctrl Pts',(-12.09839358012,36.54188398296,-4.539180913286));
#9822=CARTESIAN_POINT('Ctrl Pts',(-12.08315373025,36.56780508192,-4.972303617105));
#9823=CARTESIAN_POINT('Ctrl Pts',(-12.07454836184,36.58402752374,-5.198381379176));
#9824=CARTESIAN_POINT('Ctrl Pts',(-12.07325486239,36.58650065764,-5.231989739265));
#9825=CARTESIAN_POINT('Ctrl Pts',(-11.57215740323,37.08103820478,5.230385959406));
#9826=CARTESIAN_POINT('Ctrl Pts',(-11.57454062195,37.07967329503,5.197321349729));
#9827=CARTESIAN_POINT('Ctrl Pts',(-11.5994870504,37.06582965207,4.84877474796));
#9828=CARTESIAN_POINT('Ctrl Pts',(-11.6435586348,37.04985783468,4.182159616124));
#9829=CARTESIAN_POINT('Ctrl Pts',(-11.69565427244,37.04432452161,3.226793445503));
#9830=CARTESIAN_POINT('Ctrl Pts',(-11.73517840125,37.04764655185,2.277022744067));
#9831=CARTESIAN_POINT('Ctrl Pts',(-11.76164063188,37.05329035986,1.325879474367));
#9832=CARTESIAN_POINT('Ctrl Pts',(-11.77458379446,37.05704081854,0.3542057124591));
#9833=CARTESIAN_POINT('Ctrl Pts',(-11.77248304032,37.05638513415,-0.6338817685511));
#9834=CARTESIAN_POINT('Ctrl Pts',(-11.75551354838,37.05173459499,-1.592080100557));
#9835=CARTESIAN_POINT('Ctrl Pts',(-11.72777119266,37.04673198537,-2.466389122714));
#9836=CARTESIAN_POINT('Ctrl Pts',(-11.69419554211,37.0449333804,-3.238709200815));
#9837=CARTESIAN_POINT('Ctrl Pts',(-11.65766877891,37.0483717235,-3.92545012791));
#9838=CARTESIAN_POINT('Ctrl Pts',(-11.61956020182,37.05817876104,-4.547464782103));
#9839=CARTESIAN_POINT('Ctrl Pts',(-11.59047057424,37.07083271012,-4.974754447084));
#9840=CARTESIAN_POINT('Ctrl Pts',(-11.57453798318,37.07967479041,-5.197357036162));
#9841=CARTESIAN_POINT('Ctrl Pts',(-11.57215330547,37.08104070378,-5.230439469083));
#9842=CARTESIAN_POINT('Ctrl Pts',(-10.87374875436,36.99215251132,5.230664466127));
#9843=CARTESIAN_POINT('Ctrl Pts',(-10.87593621278,36.99232733695,5.197499918042));
#9844=CARTESIAN_POINT('Ctrl Pts',(-10.89888147716,36.99463686747,4.847977172931));
#9845=CARTESIAN_POINT('Ctrl Pts',(-10.94040447592,37.00791721721,4.180934342797));
#9846=CARTESIAN_POINT('Ctrl Pts',(-10.99139323323,37.03826963338,3.226556333087));
#9847=CARTESIAN_POINT('Ctrl Pts',(-11.03135207768,37.06970660384,2.277785886756));
#9848=CARTESIAN_POINT('Ctrl Pts',(-11.05876901198,37.09465581291,1.326858364153));
#9849=CARTESIAN_POINT('Ctrl Pts',(-11.07238957763,37.10800766965,0.3545564871127));
#9850=CARTESIAN_POINT('Ctrl Pts',(-11.07016832676,37.10578545697,-0.634482238718));
#9851=CARTESIAN_POINT('Ctrl Pts',(-11.05236940635,37.08859174469,-1.593087932742));
#9852=CARTESIAN_POINT('Ctrl Pts',(-11.02381047398,37.06348554479,-2.466967558413));
#9853=CARTESIAN_POINT('Ctrl Pts',(-10.99004459132,37.03792904407,-3.23845314518));
#9854=CARTESIAN_POINT('Ctrl Pts',(-10.9542117178,37.01614834803,-3.924505970997));
#9855=CARTESIAN_POINT('Ctrl Pts',(-10.91774690885,37.00027711191,-4.546416048914));
#9856=CARTESIAN_POINT('Ctrl Pts',(-10.89058822231,36.99380152261,-4.974309597361));
#9857=CARTESIAN_POINT('Ctrl Pts',(-10.87593384298,36.99232715763,-5.197535697532));
#9858=CARTESIAN_POINT('Ctrl Pts',(-10.87374518234,36.9921524769,-5.23071811287));
#9859=CARTESIAN_POINT('',(-12.,36.0000000009788,5.13112119227213));
#9860=CARTESIAN_POINT('',(-12.,36.0000000049393,-5.131119091281));
#9861=CARTESIAN_POINT('Ctrl Pts',(-12.,36.0000000009797,5.13112119227213));
#9862=CARTESIAN_POINT('Ctrl Pts',(-11.99999999395,35.9999998123161,4.8038301627559));
#9863=CARTESIAN_POINT('Ctrl Pts',(-12.00000000281,36.0095311616598,4.1528235072652));
#9864=CARTESIAN_POINT('Ctrl Pts',(-11.99999999925,36.03866469074,3.18892578408));
#9865=CARTESIAN_POINT('Ctrl Pts',(-12.0000000002,36.07095734545,2.231869777753));
#9866=CARTESIAN_POINT('Ctrl Pts',(-11.99999999995,36.0961909677,1.315189036053));
#9867=CARTESIAN_POINT('Ctrl Pts',(-12.00000000001,36.11044635878,0.3796003502206));
#9868=CARTESIAN_POINT('Ctrl Pts',(-12.,36.10831608628,-0.6377249666603));
#9869=CARTESIAN_POINT('Ctrl Pts',(-11.99999999999,36.08871384336,-1.625489635872));
#9870=CARTESIAN_POINT('Ctrl Pts',(-12.00000000003,36.06245143419,-2.484605093247));
#9871=CARTESIAN_POINT('Ctrl Pts',(-11.99999999989,36.03698770308,-3.246220814887));
#9872=CARTESIAN_POINT('Ctrl Pts',(-12.00000000042,36.01653250216,-3.92832252103));
#9873=CARTESIAN_POINT('Ctrl Pts',(-11.99999999844,36.003251535809,-4.54965314868712));
#9874=CARTESIAN_POINT('Ctrl Pts',(-12.00000000337,35.9999999663184,-4.94198226040701));
#9875=CARTESIAN_POINT('Ctrl Pts',(-12.0000000000001,36.0000000049386,-5.1311190912794));
#9876=CARTESIAN_POINT('Origin',(-11.,36.,5.131121190326));
#9877=CARTESIAN_POINT('Origin',(-11.,36.,-5.131119091281));
#9878=CARTESIAN_POINT('Origin',(-12.,37.,-8.));
#9879=CARTESIAN_POINT('',(-12.,36.,8.));
#9880=CARTESIAN_POINT('',(-12.,36.,8.));
#9881=CARTESIAN_POINT('',(-12.,36.,-7.));
#9882=CARTESIAN_POINT('',(-12.,36.00000000494,-5.131124034723));
#9883=CARTESIAN_POINT('',(-12.,6.,-7.));
#9884=CARTESIAN_POINT('',(-12.,6.,-7.));
#9885=CARTESIAN_POINT('',(-12.,5.999999999898,7.));
#9886=CARTESIAN_POINT('',(-12.,6.,-7.));
#9887=CARTESIAN_POINT('',(-12.,5.732050807569,8.));
#9888=CARTESIAN_POINT('Origin',(-12.,4.,7.));
#9889=CARTESIAN_POINT('',(-12.,20.,8.));
#9890=CARTESIAN_POINT('',(-12.,20.,8.));
#9891=CARTESIAN_POINT('',(-12.,20.,7.));
#9892=CARTESIAN_POINT('',(-12.,20.,8.));
#9893=CARTESIAN_POINT('',(-12.,27.,7.));
#9894=CARTESIAN_POINT('',(-12.,20.,7.));
#9895=CARTESIAN_POINT('',(-12.,27.,8.));
#9896=CARTESIAN_POINT('',(-12.,27.,8.));
#9897=CARTESIAN_POINT('',(-12.,36.,8.));
#9898=CARTESIAN_POINT('',(-12.,16.4,2.625));
#9899=CARTESIAN_POINT('Origin',(-12.,16.4,0.));
#9900=CARTESIAN_POINT('Origin',(-12.,16.4,0.));
#9901=CARTESIAN_POINT('',(-6.66390773956619,16.3999999998592,2.625));
#9902=CARTESIAN_POINT('',(-12.,16.4,2.625));
#9903=CARTESIAN_POINT('',(-6.75,15.85786437627,2.56840689250806));
#9904=CARTESIAN_POINT('Ctrl Pts',(-6.66390773956619,16.3999999997184,2.625));
#9905=CARTESIAN_POINT('Ctrl Pts',(-6.72228020467757,16.2208448358157,2.62499999998078));
#9906=CARTESIAN_POINT('Ctrl Pts',(-6.75,16.0334600508686,2.60547137432769));
#9907=CARTESIAN_POINT('Ctrl Pts',(-6.75,15.85786437627,2.56840689250806));
#9908=CARTESIAN_POINT('',(-3.336092260526,16.4,2.625));
#9909=CARTESIAN_POINT('Ctrl Pts',(-6.75,15.85786437627,2.56840689250806));
#9910=CARTESIAN_POINT('Ctrl Pts',(-6.75,15.6110066826013,2.51630052644901));
#9911=CARTESIAN_POINT('Ctrl Pts',(-6.69544690549609,15.3629337030798,2.42419944853985));
#9912=CARTESIAN_POINT('Ctrl Pts',(-6.50091953601999,14.9268772497432,2.18681464246373));
#9913=CARTESIAN_POINT('Ctrl Pts',(-6.36151207057982,14.7383593594213,2.04204903773034));
#9914=CARTESIAN_POINT('Ctrl Pts',(-6.06085872962622,14.4510762985029,1.76929702284452));
#9915=CARTESIAN_POINT('Ctrl Pts',(-5.87839362558371,14.3282234441449,1.61886205539035));
#9916=CARTESIAN_POINT('Ctrl Pts',(-5.57238612680822,14.2004286716704,1.4346071596535));
#9917=CARTESIAN_POINT('Ctrl Pts',(-5.46497331884357,14.1668647431483,1.38050334687473));
#9918=CARTESIAN_POINT('Ctrl Pts',(-5.24008283204397,14.1206143358393,1.30271393580598));
#9919=CARTESIAN_POINT('Ctrl Pts',(-5.12250669020694,14.10786437627,1.27935111772644));
#9920=CARTESIAN_POINT('Ctrl Pts',(-5.,14.10786437627,1.27935111772644));
#9921=CARTESIAN_POINT('Ctrl Pts',(-4.87749330979306,14.10786437627,1.27935111772644));
#9922=CARTESIAN_POINT('Ctrl Pts',(-4.75991716795603,14.1206143358393,1.30271393580598));
#9923=CARTESIAN_POINT('Ctrl Pts',(-4.53502668115643,14.1668647431483,1.38050334687473));
#9924=CARTESIAN_POINT('Ctrl Pts',(-4.42761387319178,14.2004286716704,1.43460715965351));
#9925=CARTESIAN_POINT('Ctrl Pts',(-4.1216063744163,14.3282234441449,1.61886205539036));
#9926=CARTESIAN_POINT('Ctrl Pts',(-3.93914127037378,14.4510762985029,1.76929702284452));
#9927=CARTESIAN_POINT('Ctrl Pts',(-3.63848792942018,14.7383593594213,2.04204903773034));
#9928=CARTESIAN_POINT('Ctrl Pts',(-3.49908046398001,14.9268772497432,2.18681464246373));
#9929=CARTESIAN_POINT('Ctrl Pts',(-3.30455309450391,15.3629337030798,2.42419944853985));
#9930=CARTESIAN_POINT('Ctrl Pts',(-3.25,15.6110066826013,2.51630052644901));
#9931=CARTESIAN_POINT('Ctrl Pts',(-3.25,16.0334600509606,2.60547137434711));
#9932=CARTESIAN_POINT('Ctrl Pts',(-3.2777197953528,16.2208448360119,2.625));
#9933=CARTESIAN_POINT('Ctrl Pts',(-3.33609226052561,16.4000000000001,2.625));
#9934=CARTESIAN_POINT('',(-3.,16.4,2.625));
#9935=CARTESIAN_POINT('',(-12.,16.4,2.625));
#9936=CARTESIAN_POINT('Origin',(-3.,16.4,0.));
#9937=CARTESIAN_POINT('Ctrl Pts',(-3.33609226052562,16.4000000000001,2.625));
#9938=CARTESIAN_POINT('Ctrl Pts',(-3.3492132620138,16.4402706167429,2.625));
#9939=CARTESIAN_POINT('Ctrl Pts',(-3.36382529489561,16.4801444941516,2.62407088270354));
#9940=CARTESIAN_POINT('Ctrl Pts',(-3.46726090935699,16.733454192834,2.61253457823639));
#9941=CARTESIAN_POINT('Ctrl Pts',(-3.59948380965172,16.9291453900179,2.57606325080576));
#9942=CARTESIAN_POINT('Ctrl Pts',(-3.90599376649975,17.2416586072539,2.49181760818345));
#9943=CARTESIAN_POINT('Ctrl Pts',(-4.10241398861631,17.3784789139656,2.43788036890531));
#9944=CARTESIAN_POINT('Ctrl Pts',(-4.53619933463474,17.5616298280266,2.35611948220898));
#9945=CARTESIAN_POINT('Ctrl Pts',(-4.77403581009751,17.60786437627,2.33059834560524));
#9946=CARTESIAN_POINT('Ctrl Pts',(-5.22596418990249,17.60786437627,2.33059834560524));
#9947=CARTESIAN_POINT('Ctrl Pts',(-5.46380066536526,17.5616298280266,2.35611948220898));
#9948=CARTESIAN_POINT('Ctrl Pts',(-5.89758601138369,17.3784789139656,2.43788036890531));
#9949=CARTESIAN_POINT('Ctrl Pts',(-6.09400623350025,17.2416586072539,2.49181760818345));
#9950=CARTESIAN_POINT('Ctrl Pts',(-6.40051619034828,16.9291453900179,2.57606325080576));
#9951=CARTESIAN_POINT('Ctrl Pts',(-6.53273909064301,16.733454192834,2.61253457823639));
#9952=CARTESIAN_POINT('Ctrl Pts',(-6.63617470514179,16.48014449406,2.62407088270771));
#9953=CARTESIAN_POINT('Ctrl Pts',(-6.65078673805434,16.4402706165569,2.62500000000432));
#9954=CARTESIAN_POINT('Ctrl Pts',(-6.66390773956619,16.3999999997184,2.625));
#9955=CARTESIAN_POINT('Origin',(-3.,0.,-8.));
#9956=CARTESIAN_POINT('Origin',(-5.,15.85786437627,8.));
#9957=CARTESIAN_POINT('',(-6.75,15.85786437627,8.));
#9958=CARTESIAN_POINT('',(-6.75,15.85786437627,8.));
#9959=CARTESIAN_POINT('Origin',(-5.,15.85786437627,8.));
#9960=CARTESIAN_POINT('Origin',(0.,0.,8.));
#9961=CARTESIAN_POINT('',(-11.,37.,8.));
#9962=CARTESIAN_POINT('Origin',(-11.,36.,8.));
#9963=CARTESIAN_POINT('',(12.,27.,8.));
#9964=CARTESIAN_POINT('',(-12.,27.,8.));
#9965=CARTESIAN_POINT('',(12.,36.,8.));
#9966=CARTESIAN_POINT('',(12.,27.,8.));
#9967=CARTESIAN_POINT('',(11.,37.,8.));
#9968=CARTESIAN_POINT('Origin',(11.,36.,8.));
#9969=CARTESIAN_POINT('',(6.,37.,8.));
#9970=CARTESIAN_POINT('',(6.,37.,8.));
#9971=CARTESIAN_POINT('',(-2.,30.,8.));
#9972=CARTESIAN_POINT('Origin',(0.,30.,8.));
#9973=CARTESIAN_POINT('Origin',(0.,0.,8.));
#9974=CARTESIAN_POINT('',(12.,5.732050807569,8.));
#9975=CARTESIAN_POINT('',(12.,20.,8.));
#9976=CARTESIAN_POINT('',(12.,5.732050807569,8.));
#9977=CARTESIAN_POINT('',(-12.,20.,8.));
#9978=CARTESIAN_POINT('',(-13.,4.,8.));
#9979=CARTESIAN_POINT('Ctrl Pts',(-13.,4.,8.));
#9980=CARTESIAN_POINT('Ctrl Pts',(-12.722901777919,4.27709822208096,8.));
#9981=CARTESIAN_POINT('Ctrl Pts',(-12.3960872838113,4.61522327220401,8.));
#9982=CARTESIAN_POINT('Ctrl Pts',(-12.0895719998978,5.18473047315088,8.));
#9983=CARTESIAN_POINT('Ctrl Pts',(-12.,5.47717338569331,8.));
#9984=CARTESIAN_POINT('Ctrl Pts',(-12.,5.73205080756888,8.));
#9985=CARTESIAN_POINT('',(-20.,4.,8.));
#9986=CARTESIAN_POINT('',(-13.,4.,8.));
#9987=CARTESIAN_POINT('',(-20.,0.,8.));
#9988=CARTESIAN_POINT('',(-20.,4.,8.));
#9989=CARTESIAN_POINT('',(20.,0.,8.));
#9990=CARTESIAN_POINT('',(-20.,0.,8.));
#9991=CARTESIAN_POINT('',(20.,4.,8.));
#9992=CARTESIAN_POINT('',(20.,0.,8.));
#9993=CARTESIAN_POINT('',(13.,4.,8.));
#9994=CARTESIAN_POINT('',(20.,4.,8.));
#9995=CARTESIAN_POINT('Ctrl Pts',(12.,5.73205080756888,8.));
#9996=CARTESIAN_POINT('Ctrl Pts',(12.,5.47717338569331,8.));
#9997=CARTESIAN_POINT('Ctrl Pts',(12.0895719998978,5.18473047315088,8.));
#9998=CARTESIAN_POINT('Ctrl Pts',(12.3960872838113,4.61522327220401,8.));
#9999=CARTESIAN_POINT('Ctrl Pts',(12.722901777919,4.27709822208096,8.));
#10000=CARTESIAN_POINT('Ctrl Pts',(13.,4.,8.));
#10001=CARTESIAN_POINT('',(3.25,15.85786437627,8.));
#10002=CARTESIAN_POINT('Origin',(5.,15.85786437627,8.));
#10003=CARTESIAN_POINT('Origin',(5.,15.85786437627,8.));
#10004=CARTESIAN_POINT('',(6.75,15.85786437627,2.568406892508));
#10005=CARTESIAN_POINT('',(3.25,15.85786437627,2.56840689250806));
#10006=CARTESIAN_POINT('Ctrl Pts',(6.75,15.85786437627,2.56840689250806));
#10007=CARTESIAN_POINT('Ctrl Pts',(6.75,15.6110066826013,2.51630052644901));
#10008=CARTESIAN_POINT('Ctrl Pts',(6.69544690549608,15.3629337030798,2.42419944853985));
#10009=CARTESIAN_POINT('Ctrl Pts',(6.50091953601999,14.9268772497432,2.18681464246373));
#10010=CARTESIAN_POINT('Ctrl Pts',(6.36151207057982,14.7383593594213,2.04204903773034));
#10011=CARTESIAN_POINT('Ctrl Pts',(6.06085872962622,14.4510762985029,1.76929702284452));
#10012=CARTESIAN_POINT('Ctrl Pts',(5.8783936255837,14.3282234441449,1.61886205539036));
#10013=CARTESIAN_POINT('Ctrl Pts',(5.57238612680822,14.2004286716704,1.43460715965351));
#10014=CARTESIAN_POINT('Ctrl Pts',(5.46497331884357,14.1668647431483,1.38050334687473));
#10015=CARTESIAN_POINT('Ctrl Pts',(5.24008283204397,14.1206143358393,1.30271393580598));
#10016=CARTESIAN_POINT('Ctrl Pts',(5.12250669020694,14.10786437627,1.27935111772644));
#10017=CARTESIAN_POINT('Ctrl Pts',(5.,14.10786437627,1.27935111772644));
#10018=CARTESIAN_POINT('Ctrl Pts',(4.87749330979306,14.10786437627,1.27935111772644));
#10019=CARTESIAN_POINT('Ctrl Pts',(4.75991716795603,14.1206143358393,1.30271393580598));
#10020=CARTESIAN_POINT('Ctrl Pts',(4.53502668115643,14.1668647431483,1.38050334687473));
#10021=CARTESIAN_POINT('Ctrl Pts',(4.42761387319178,14.2004286716704,1.43460715965351));
#10022=CARTESIAN_POINT('Ctrl Pts',(4.1216063744163,14.3282234441449,1.61886205539036));
#10023=CARTESIAN_POINT('Ctrl Pts',(3.93914127037378,14.4510762985029,1.76929702284452));
#10024=CARTESIAN_POINT('Ctrl Pts',(3.63848792942018,14.7383593594213,2.04204903773034));
#10025=CARTESIAN_POINT('Ctrl Pts',(3.49908046398001,14.9268772497432,2.18681464246373));
#10026=CARTESIAN_POINT('Ctrl Pts',(3.30455309450391,15.3629337030798,2.42419944853985));
#10027=CARTESIAN_POINT('Ctrl Pts',(3.25,15.6110066826013,2.51630052644901));
#10028=CARTESIAN_POINT('Ctrl Pts',(3.25,15.85786437627,2.56840689250806));
#10029=CARTESIAN_POINT('',(3.25,15.85786437627,8.));
#10030=CARTESIAN_POINT('',(3.33609226043381,16.3999999998592,2.625));
#10031=CARTESIAN_POINT('Ctrl Pts',(3.25,15.85786437627,2.56840689250806));
#10032=CARTESIAN_POINT('Ctrl Pts',(3.25,16.0334600508686,2.60547137432769));
#10033=CARTESIAN_POINT('Ctrl Pts',(3.27771979532244,16.2208448358157,2.62499999998078));
#10034=CARTESIAN_POINT('Ctrl Pts',(3.33609226043381,16.3999999997184,2.625));
#10035=CARTESIAN_POINT('',(6.66390773956619,16.3999999998592,2.625));
#10036=CARTESIAN_POINT('Ctrl Pts',(3.33609226043381,16.3999999997184,2.625));
#10037=CARTESIAN_POINT('Ctrl Pts',(3.34921326194566,16.4402706165569,2.62500000000432));
#10038=CARTESIAN_POINT('Ctrl Pts',(3.36382529485821,16.48014449406,2.62407088270771));
#10039=CARTESIAN_POINT('Ctrl Pts',(3.46726090935699,16.733454192834,2.61253457823639));
#10040=CARTESIAN_POINT('Ctrl Pts',(3.59948380965172,16.9291453900179,2.57606325080576));
#10041=CARTESIAN_POINT('Ctrl Pts',(3.90599376649975,17.2416586072539,2.49181760818345));
#10042=CARTESIAN_POINT('Ctrl Pts',(4.10241398861631,17.3784789139656,2.43788036890531));
#10043=CARTESIAN_POINT('Ctrl Pts',(4.53619933463474,17.5616298280266,2.35611948220898));
#10044=CARTESIAN_POINT('Ctrl Pts',(4.77403581009751,17.60786437627,2.33059834560524));
#10045=CARTESIAN_POINT('Ctrl Pts',(5.22596418990249,17.60786437627,2.33059834560524));
#10046=CARTESIAN_POINT('Ctrl Pts',(5.46380066536526,17.5616298280266,2.35611948220898));
#10047=CARTESIAN_POINT('Ctrl Pts',(5.89758601138369,17.3784789139656,2.43788036890531));
#10048=CARTESIAN_POINT('Ctrl Pts',(6.09400623350025,17.2416586072539,2.49181760818345));
#10049=CARTESIAN_POINT('Ctrl Pts',(6.40051619034828,16.9291453900179,2.57606325080576));
#10050=CARTESIAN_POINT('Ctrl Pts',(6.53273909064301,16.733454192834,2.61253457823639));
#10051=CARTESIAN_POINT('Ctrl Pts',(6.63617470514179,16.48014449406,2.62407088270771));
#10052=CARTESIAN_POINT('Ctrl Pts',(6.65078673805434,16.4402706165569,2.62500000000432));
#10053=CARTESIAN_POINT('Ctrl Pts',(6.66390773956619,16.3999999997184,2.625));
#10054=CARTESIAN_POINT('Ctrl Pts',(6.66390773956619,16.3999999997184,2.625));
#10055=CARTESIAN_POINT('Ctrl Pts',(6.72228020467757,16.2208448358157,2.62499999998078));
#10056=CARTESIAN_POINT('Ctrl Pts',(6.75,16.0334600508686,2.60547137432769));
#10057=CARTESIAN_POINT('Ctrl Pts',(6.75,15.85786437627,2.56840689250806));
#10058=CARTESIAN_POINT('Origin',(12.,16.4,0.));
#10059=CARTESIAN_POINT('',(3.,16.4,2.625));
#10060=CARTESIAN_POINT('Origin',(3.,16.4,0.));
#10061=CARTESIAN_POINT('',(12.,16.4,2.625));
#10062=CARTESIAN_POINT('',(12.,16.4,2.625));
#10063=CARTESIAN_POINT('',(12.,16.4,2.625));
#10064=CARTESIAN_POINT('Origin',(12.,16.4,0.));
#10065=CARTESIAN_POINT('Origin',(12.,5.,-8.));
#10066=CARTESIAN_POINT('',(12.,6.,-7.));
#10067=CARTESIAN_POINT('',(12.,5.999999999485,7.));
#10068=CARTESIAN_POINT('',(12.,6.,-7.));
#10069=CARTESIAN_POINT('',(12.,36.,-7.));
#10070=CARTESIAN_POINT('',(12.,36.,-7.));
#10071=CARTESIAN_POINT('',(12.,36.,-5.13112138723605));
#10072=CARTESIAN_POINT('',(12.,36.,-5.131121557209));
#10073=CARTESIAN_POINT('',(11.9999999999999,36.10888778104,-0.00016660306200075));
#10074=CARTESIAN_POINT('Ctrl Pts',(12.,36.10888778104,-0.0001666008893355));
#10075=CARTESIAN_POINT('Ctrl Pts',(12.,36.10888720385,-0.2115948044887));
#10076=CARTESIAN_POINT('Ctrl Pts',(12.,36.10647748554,-0.632542946972));
#10077=CARTESIAN_POINT('Ctrl Pts',(12.,36.09662552275,-1.246846637783));
#10078=CARTESIAN_POINT('Ctrl Pts',(12.,36.08098057782,-1.878213676881));
#10079=CARTESIAN_POINT('Ctrl Pts',(12.,36.06231044761,-2.484098080739));
#10080=CARTESIAN_POINT('Ctrl Pts',(12.,36.04274891785,-3.075021505576));
#10081=CARTESIAN_POINT('Ctrl Pts',(12.,36.02306872989,-3.696652254043));
#10082=CARTESIAN_POINT('Ctrl Pts',(12.,36.0059704833598,-4.37191141631148));
#10083=CARTESIAN_POINT('Ctrl Pts',(12.,35.9999999979788,-4.87066496985907));
#10084=CARTESIAN_POINT('Ctrl Pts',(12.,36.,-5.13112138723605));
#10085=CARTESIAN_POINT('',(12.,36.0000000210414,5.1311211680071));
#10086=CARTESIAN_POINT('Ctrl Pts',(11.9999999999999,36.00000002104,5.13112116800713));
#10087=CARTESIAN_POINT('Ctrl Pts',(11.99999997181,36.0000000085565,4.8397925008905));
#10088=CARTESIAN_POINT('Ctrl Pts',(12.00000001305,36.0075844610583,4.27293018632732));
#10089=CARTESIAN_POINT('Ctrl Pts',(11.99999999661,36.0287089676,3.502562898396));
#10090=CARTESIAN_POINT('Ctrl Pts',(12.00000000053,36.05480007394,2.714420520144));
#10091=CARTESIAN_POINT('Ctrl Pts',(12.00000000128,36.08110280775,1.891087904674));
#10092=CARTESIAN_POINT('Ctrl Pts',(11.99999999435,36.1023071011,1.013181682868));
#10093=CARTESIAN_POINT('Ctrl Pts',(12.00000001234,36.10888952645,0.3484660678232));
#10094=CARTESIAN_POINT('Ctrl Pts',(12.,36.10888778104,-0.0001666008893355));
#10095=CARTESIAN_POINT('',(12.,36.,8.));
#10096=CARTESIAN_POINT('',(12.,27.,7.));
#10097=CARTESIAN_POINT('',(12.,27.,8.));
#10098=CARTESIAN_POINT('',(12.,20.,7.));
#10099=CARTESIAN_POINT('',(12.,20.,7.));
#10100=CARTESIAN_POINT('',(12.,20.,8.));
#10101=CARTESIAN_POINT('Origin',(12.,4.,7.));
#10102=CARTESIAN_POINT('Origin',(3.,0.,-8.));
#10103=CARTESIAN_POINT('Origin',(13.,6.,-43.78380184031));
#10104=CARTESIAN_POINT('',(13.,5.,7.));
#10105=CARTESIAN_POINT('Origin',(13.,6.,7.));
#10106=CARTESIAN_POINT('',(13.,5.,0.));
#10107=CARTESIAN_POINT('',(13.,5.,0.));
#10108=CARTESIAN_POINT('',(13.,5.,-7.));
#10109=CARTESIAN_POINT('',(13.,5.,-7.));
#10110=CARTESIAN_POINT('Origin',(13.,6.,-7.));
#10111=CARTESIAN_POINT('Origin',(13.,6.,-7.));
#10112=CARTESIAN_POINT('',(11.,6.,-8.));
#10113=CARTESIAN_POINT('',(13.,4.,-8.));
#10114=CARTESIAN_POINT('Origin',(13.,6.,-8.));
#10115=CARTESIAN_POINT('Origin',(11.,6.,-7.));
#10116=CARTESIAN_POINT('Origin',(13.,4.,-7.));
#10117=CARTESIAN_POINT('Origin',(0.,0.,-8.));
#10118=CARTESIAN_POINT('',(-11.,6.,-8.));
#10119=CARTESIAN_POINT('',(-11.,37.,-8.));
#10120=CARTESIAN_POINT('',(-11.,6.,-8.));
#10121=CARTESIAN_POINT('',(6.,37.,-8.));
#10122=CARTESIAN_POINT('',(11.,37.,-8.));
#10123=CARTESIAN_POINT('',(6.,37.,-8.));
#10124=CARTESIAN_POINT('',(11.,37.,-8.));
#10125=CARTESIAN_POINT('',(20.,4.,-8.));
#10126=CARTESIAN_POINT('',(13.,4.,-8.));
#10127=CARTESIAN_POINT('',(20.,0.,-8.));
#10128=CARTESIAN_POINT('',(20.,4.,-8.));
#10129=CARTESIAN_POINT('',(-20.,0.,-8.));
#10130=CARTESIAN_POINT('',(-20.,0.,-8.));
#10131=CARTESIAN_POINT('',(-20.,4.,-8.));
#10132=CARTESIAN_POINT('',(-20.,0.,-8.));
#10133=CARTESIAN_POINT('',(-13.,4.,-8.));
#10134=CARTESIAN_POINT('',(-20.,4.,-8.));
#10135=CARTESIAN_POINT('Origin',(-13.,6.,-8.));
#10136=CARTESIAN_POINT('',(-2.,30.,-8.));
#10137=CARTESIAN_POINT('Origin',(0.,30.,-8.));
#10138=CARTESIAN_POINT('Origin',(0.,30.,-8.));
#10139=CARTESIAN_POINT('',(-2.,30.,-8.));
#10140=CARTESIAN_POINT('Origin',(-11.,-152.5212,-7.));
#10141=CARTESIAN_POINT('Origin',(-11.,6.,-7.));
#10142=CARTESIAN_POINT('Origin',(-11.,36.,-7.));
#10143=CARTESIAN_POINT('Origin',(-11.,36.,8.15648));
#10144=CARTESIAN_POINT('',(-11.00000012291,37.,-5.131119600082));
#10145=CARTESIAN_POINT('Origin',(12.,37.,-8.));
#10146=CARTESIAN_POINT('',(-11.,37.,8.));
#10147=CARTESIAN_POINT('Origin',(12.,37.,-8.));
#10148=CARTESIAN_POINT('Origin',(12.,37.,-8.));
#10149=CARTESIAN_POINT('',(11.,37.,8.));
#10150=CARTESIAN_POINT('Origin',(12.,37.,-8.));
#10151=CARTESIAN_POINT('',(11.00000000411,37.,-5.131121402775));
#10152=CARTESIAN_POINT('Origin',(-11.,36.,43.78380184031));
#10153=CARTESIAN_POINT('Origin',(11.,36.,43.78380184031));
#10154=CARTESIAN_POINT('Origin',(11.,36.,5.131121166588));
#10155=CARTESIAN_POINT('Ctrl Pts',(10.87639820398,36.99238627919,5.190418362005));
#10156=CARTESIAN_POINT('Ctrl Pts',(10.87769651652,36.99251157435,5.170658557952));
#10157=CARTESIAN_POINT('Ctrl Pts',(10.89692694025,36.99460171349,4.877137850237));
#10158=CARTESIAN_POINT('Ctrl Pts',(10.9315020989,37.0047000695,4.325352885477));
#10159=CARTESIAN_POINT('Ctrl Pts',(10.97577779548,37.02831631823,3.528331623006));
#10160=CARTESIAN_POINT('Ctrl Pts',(11.01326259241,37.05497526794,2.729327118972));
#10161=CARTESIAN_POINT('Ctrl Pts',(11.04382137072,37.08079008034,1.88909513595));
#10162=CARTESIAN_POINT('Ctrl Pts',(11.06541962492,37.10108731992,0.9746583446556));
#10163=CARTESIAN_POINT('Ctrl Pts',(11.07091432789,37.10655625449,0.3159910511012));
#10164=CARTESIAN_POINT('Ctrl Pts',(11.07072948767,37.10637175836,-0.04163617506052));
#10165=CARTESIAN_POINT('Ctrl Pts',(11.07070810544,37.10635038289,-0.06236933689121));
#10166=CARTESIAN_POINT('Ctrl Pts',(11.57504126409,37.07940693165,5.190257582826));
#10167=CARTESIAN_POINT('Ctrl Pts',(11.57645336605,37.07861826856,5.170553848682));
#10168=CARTESIAN_POINT('Ctrl Pts',(11.59734297401,37.06717003218,4.87782845147));
#10169=CARTESIAN_POINT('Ctrl Pts',(11.63415546378,37.0529119173,4.326540263707));
#10170=CARTESIAN_POINT('Ctrl Pts',(11.67980309249,37.04535955746,3.528923029992));
#10171=CARTESIAN_POINT('Ctrl Pts',(11.71737756968,37.04564363316,2.72899893329));
#10172=CARTESIAN_POINT('Ctrl Pts',(11.74726727952,37.04995202718,1.888155892492));
#10173=CARTESIAN_POINT('Ctrl Pts',(11.76797944015,37.05503499255,0.9738259564121));
#10174=CARTESIAN_POINT('Ctrl Pts',(11.77318315821,37.05662938656,0.3157193840525));
#10175=CARTESIAN_POINT('Ctrl Pts',(11.77300787451,37.05657527129,-0.04160039065528));
#10176=CARTESIAN_POINT('Ctrl Pts',(11.77298757863,37.0565689799,-0.06231576499393));
#10177=CARTESIAN_POINT('Ctrl Pts',(12.0748185662,36.58352740788,5.191173770148));
#10178=CARTESIAN_POINT('Ctrl Pts',(12.07558184615,36.58208430631,5.171161356908));
#10179=CARTESIAN_POINT('Ctrl Pts',(12.08684498807,36.56096809879,4.873900518236));
#10180=CARTESIAN_POINT('Ctrl Pts',(12.10588924084,36.53002481672,4.315495143085));
#10181=CARTESIAN_POINT('Ctrl Pts',(12.12786170733,36.50231553734,3.511843211855));
#10182=CARTESIAN_POINT('Ctrl Pts',(12.14473054851,36.48628864437,2.710134870967));
#10183=CARTESIAN_POINT('Ctrl Pts',(12.15728217879,36.47775237489,1.87171629668));
#10184=CARTESIAN_POINT('Ctrl Pts',(12.16548507289,36.47397603557,0.9640221888825));
#10185=CARTESIAN_POINT('Ctrl Pts',(12.16746589788,36.47334779007,0.3125390240587));
#10186=CARTESIAN_POINT('Ctrl Pts',(12.16739888806,36.47336841638,-0.04118134654457));
#10187=CARTESIAN_POINT('Ctrl Pts',(12.16739110543,36.47337076861,-0.06168816472244));
#10188=CARTESIAN_POINT('Ctrl Pts',(11.9932691391,35.88422585437,5.192465799906));
#10189=CARTESIAN_POINT('Ctrl Pts',(11.99311750496,35.8828886515,5.172016179191));
#10190=CARTESIAN_POINT('Ctrl Pts',(11.99083530679,35.86337341576,4.86835995167));
#10191=CARTESIAN_POINT('Ctrl Pts',(11.98570312504,35.83618480774,4.300669943404));
#10192=CARTESIAN_POINT('Ctrl Pts',(11.97707105556,35.8147556383,3.490162717829));
#10193=CARTESIAN_POINT('Ctrl Pts',(11.96828419718,35.80496385934,2.687170896915));
#10194=CARTESIAN_POINT('Ctrl Pts',(11.9600969239,35.80207422425,1.852356959427));
#10195=CARTESIAN_POINT('Ctrl Pts',(11.95374025469,35.80257324593,0.9527495005316));
#10196=CARTESIAN_POINT('Ctrl Pts',(11.95203263857,35.80307516529,0.3088837822729));
#10197=CARTESIAN_POINT('Ctrl Pts',(11.95208976203,35.80305769695,-0.04069972159253));
#10198=CARTESIAN_POINT('Ctrl Pts',(11.95209634362,35.80305563768,-0.06096681520975));
#10199=CARTESIAN_POINT('Origin',(11.,36.10888778108,-0.0001666050799347));
#10200=CARTESIAN_POINT('Ctrl Pts',(10.88028304336,37.1015617965,0.123806950294));
#10201=CARTESIAN_POINT('Ctrl Pts',(10.88028304336,37.10165143422,0.08248224247726));
#10202=CARTESIAN_POINT('Ctrl Pts',(10.88028304336,37.1019259464,-0.1723252126584));
#10203=CARTESIAN_POINT('Ctrl Pts',(10.88028304336,37.09933054386,-0.6372922628576));
#10204=CARTESIAN_POINT('Ctrl Pts',(10.88028304336,37.08914764459,-1.271464818044));
#10205=CARTESIAN_POINT('Ctrl Pts',(10.88028304336,37.07366901929,-1.89602670484));
#10206=CARTESIAN_POINT('Ctrl Pts',(10.88028304336,37.05480294858,-2.51029661392));
#10207=CARTESIAN_POINT('Ctrl Pts',(10.88028304336,37.03456745556,-3.12121065189));
#10208=CARTESIAN_POINT('Ctrl Pts',(10.88028304336,37.01469479526,-3.751183702533));
#10209=CARTESIAN_POINT('Ctrl Pts',(10.88028304336,36.99796087928,-4.424629516724));
#10210=CARTESIAN_POINT('Ctrl Pts',(10.88028304336,36.99258729792,-4.908935980834));
#10211=CARTESIAN_POINT('Ctrl Pts',(10.88028304336,36.99282614041,-5.170754488191));
#10212=CARTESIAN_POINT('Ctrl Pts',(10.88028304336,36.99286279613,-5.190561784574));
#10213=CARTESIAN_POINT('Ctrl Pts',(11.57926121074,37.18584731036,0.1239869276598));
#10214=CARTESIAN_POINT('Ctrl Pts',(11.57926121074,37.18593708415,0.08260222517352));
#10215=CARTESIAN_POINT('Ctrl Pts',(11.57926121074,37.18621200725,-0.1725758878834));
#10216=CARTESIAN_POINT('Ctrl Pts',(11.57926121074,37.18361272676,-0.638219248976));
#10217=CARTESIAN_POINT('Ctrl Pts',(11.57926121074,37.17341622784,-1.273216845643));
#10218=CARTESIAN_POINT('Ctrl Pts',(11.57926121074,37.15792160269,-1.898406858163));
#10219=CARTESIAN_POINT('Ctrl Pts',(11.57926121074,37.13904415592,-2.513037048283));
#10220=CARTESIAN_POINT('Ctrl Pts',(11.57926121074,37.11880713331,-3.123995722929));
#10221=CARTESIAN_POINT('Ctrl Pts',(11.57926121074,37.0989454502,-3.75363319921));
#10222=CARTESIAN_POINT('Ctrl Pts',(11.57926121074,37.08223377732,-4.426235196415));
#10223=CARTESIAN_POINT('Ctrl Pts',(11.57926121074,37.07687356091,-4.90952025416));
#10224=CARTESIAN_POINT('Ctrl Pts',(11.57926121074,37.0771118124,-5.170651184102));
#10225=CARTESIAN_POINT('Ctrl Pts',(11.57926121074,37.07714837518,-5.190405681367));
#10226=CARTESIAN_POINT('Ctrl Pts',(12.0770937892,36.68801592067,0.1229238934798));
#10227=CARTESIAN_POINT('Ctrl Pts',(12.0770937892,36.68810489079,0.08189354879861));
#10228=CARTESIAN_POINT('Ctrl Pts',(12.0770937892,36.68837738675,-0.1710952776352));
#10229=CARTESIAN_POINT('Ctrl Pts',(12.0770937892,36.68580101136,-0.632744016443));
#10230=CARTESIAN_POINT('Ctrl Pts',(12.0770937892,36.6756848386,-1.262868515376));
#10231=CARTESIAN_POINT('Ctrl Pts',(12.0770937892,36.66028471638,-1.884348510744));
#10232=CARTESIAN_POINT('Ctrl Pts',(12.0770937892,36.64147446212,-2.496850705164));
#10233=CARTESIAN_POINT('Ctrl Pts',(12.0770937892,36.62124647408,-3.107545733809));
#10234=CARTESIAN_POINT('Ctrl Pts',(12.0770937892,36.60131995433,-3.739165276085));
#10235=CARTESIAN_POINT('Ctrl Pts',(12.0770937892,36.58447690284,-4.416751268335));
#10236=CARTESIAN_POINT('Ctrl Pts',(12.0770937892,36.57903774649,-4.906069250679));
#10237=CARTESIAN_POINT('Ctrl Pts',(12.0770937892,36.57927948871,-5.171261348479));
#10238=CARTESIAN_POINT('Ctrl Pts',(12.0770937892,36.57931660044,-5.19132770311));
#10239=CARTESIAN_POINT('Ctrl Pts',(11.9928080612,35.98903943522,0.1214313481916));
#10240=CARTESIAN_POINT('Ctrl Pts',(11.9928080612,35.98912727695,0.0808985369691));
#10241=CARTESIAN_POINT('Ctrl Pts',(11.9928080612,35.98939636512,-0.1690164377528));
#10242=CARTESIAN_POINT('Ctrl Pts',(11.9928080612,35.98685214946,-0.6250565566483));
#10243=CARTESIAN_POINT('Ctrl Pts',(11.9928080612,35.97684875804,-1.248339018703));
#10244=CARTESIAN_POINT('Ctrl Pts',(11.9928080612,35.96158132197,-1.864609991895));
#10245=CARTESIAN_POINT('Ctrl Pts',(11.9928080612,35.94286540886,-2.474124389668));
#10246=CARTESIAN_POINT('Ctrl Pts',(11.9928080612,35.92265010573,-3.084449248094));
#10247=CARTESIAN_POINT('Ctrl Pts',(11.9928080612,35.90263255259,-3.718851695488));
#10248=CARTESIAN_POINT('Ctrl Pts',(11.9928080612,35.88560503994,-4.403435429169));
#10249=CARTESIAN_POINT('Ctrl Pts',(11.9928080612,35.88005504854,-4.901223894733));
#10250=CARTESIAN_POINT('Ctrl Pts',(11.9928080612,35.8803016919,-5.172118045266));
#10251=CARTESIAN_POINT('Ctrl Pts',(11.9928080612,35.88033957438,-5.192622260927));
#10252=CARTESIAN_POINT('Origin',(11.,36.,-5.131121385248));
#10253=CARTESIAN_POINT('Origin',(11.,36.,8.15648));
#10254=CARTESIAN_POINT('Origin',(11.,36.,-7.));
#10255=CARTESIAN_POINT('Origin',(11.,266.1186496051,-7.));
#10256=CARTESIAN_POINT('Origin',(-13.,6.,-7.));
#10257=CARTESIAN_POINT('',(-13.,5.,-7.));
#10258=CARTESIAN_POINT('Origin',(-13.,4.,-7.));
#10259=CARTESIAN_POINT('Origin',(-13.,6.,-7.));
#10260=CARTESIAN_POINT('Origin',(-13.,6.,-43.78380184031));
#10261=CARTESIAN_POINT('',(-13.,5.,0.));
#10262=CARTESIAN_POINT('',(-13.,5.,-7.));
#10263=CARTESIAN_POINT('',(-13.,5.,7.));
#10264=CARTESIAN_POINT('',(-13.,5.,-1.571160412673E-14));
#10265=CARTESIAN_POINT('Origin',(-13.,6.,7.));
#10266=CARTESIAN_POINT('Origin',(-12.,5.,-8.));
#10267=CARTESIAN_POINT('',(-17.,5.,2.44929359829471E-16));
#10268=CARTESIAN_POINT('Origin',(-15.,5.,0.));
#10269=CARTESIAN_POINT('',(-20.,5.,-7.));
#10270=CARTESIAN_POINT('',(-20.,5.,-7.));
#10271=CARTESIAN_POINT('',(-20.,5.,7.));
#10272=CARTESIAN_POINT('',(-20.,5.,7.));
#10273=CARTESIAN_POINT('',(-13.,5.,7.));
#10274=CARTESIAN_POINT('Origin',(-15.,5.,0.));
#10275=CARTESIAN_POINT('Origin',(-15.,5.,0.));
#10276=CARTESIAN_POINT('',(-17.,0.,0.));
#10277=CARTESIAN_POINT('Origin',(-15.,0.,0.));
#10278=CARTESIAN_POINT('',(-17.,5.,2.44929359829471E-16));
#10279=CARTESIAN_POINT('Origin',(-21.,0.,-8.));
#10280=CARTESIAN_POINT('',(-21.,0.,7.));
#10281=CARTESIAN_POINT('Origin',(-20.,0.,7.));
#10282=CARTESIAN_POINT('',(-21.,0.,-7.));
#10283=CARTESIAN_POINT('',(-21.,0.,-7.));
#10284=CARTESIAN_POINT('Origin',(-20.,0.,-7.));
#10285=CARTESIAN_POINT('',(21.,0.,-7.));
#10286=CARTESIAN_POINT('Origin',(20.,0.,-7.));
#10287=CARTESIAN_POINT('',(21.,0.,7.));
#10288=CARTESIAN_POINT('',(21.,0.,-7.));
#10289=CARTESIAN_POINT('Origin',(20.,0.,7.));
#10290=CARTESIAN_POINT('',(13.,0.,0.));
#10291=CARTESIAN_POINT('Origin',(15.,0.,0.));
#10292=CARTESIAN_POINT('Origin',(15.,5.,0.));
#10293=CARTESIAN_POINT('',(13.,5.,2.44929359829471E-16));
#10294=CARTESIAN_POINT('Origin',(15.,5.,0.));
#10295=CARTESIAN_POINT('Origin',(21.,5.,-8.));
#10296=CARTESIAN_POINT('',(20.,5.,7.));
#10297=CARTESIAN_POINT('',(20.,5.,7.));
#10298=CARTESIAN_POINT('',(20.,5.,-7.));
#10299=CARTESIAN_POINT('',(20.,5.,7.));
#10300=CARTESIAN_POINT('',(13.,5.,-7.));
#10301=CARTESIAN_POINT('Origin',(-75.7512,4.,-7.));
#10302=CARTESIAN_POINT('Origin',(20.,4.,-7.));
#10303=CARTESIAN_POINT('Origin',(20.,4.,-7.));
#10304=CARTESIAN_POINT('',(21.,4.,-7.));
#10305=CARTESIAN_POINT('Origin',(20.,4.,-7.));
#10306=CARTESIAN_POINT('Origin',(20.,4.,-7.));
#10307=CARTESIAN_POINT('Origin',(20.,243.2441960567,-7.));
#10308=CARTESIAN_POINT('',(21.,4.,-7.));
#10309=CARTESIAN_POINT('Origin',(21.,0.,-8.));
#10310=CARTESIAN_POINT('',(21.,4.,7.));
#10311=CARTESIAN_POINT('',(21.,0.,7.));
#10312=CARTESIAN_POINT('',(21.,4.,7.));
#10313=CARTESIAN_POINT('Origin',(20.,-152.5212,7.));
#10314=CARTESIAN_POINT('Origin',(20.,4.,7.));
#10315=CARTESIAN_POINT('Origin',(20.,4.,7.));
#10316=CARTESIAN_POINT('Origin',(20.,4.,7.));
#10317=CARTESIAN_POINT('Origin',(20.,4.,7.));
#10318=CARTESIAN_POINT('Origin',(75.7512,4.,7.));
#10319=CARTESIAN_POINT('Origin',(13.,4.,7.));
#10320=CARTESIAN_POINT('Origin',(13.,4.,7.));
#10321=CARTESIAN_POINT('Origin',(20.,4.,43.78380184031));
#10322=CARTESIAN_POINT('Origin',(-20.,257.4707560608,7.));
#10323=CARTESIAN_POINT('',(-21.,4.,7.));
#10324=CARTESIAN_POINT('Origin',(-20.,4.,7.));
#10325=CARTESIAN_POINT('',(-21.,4.,7.));
#10326=CARTESIAN_POINT('Origin',(-21.,5.,-8.));
#10327=CARTESIAN_POINT('',(-21.,4.,-7.));
#10328=CARTESIAN_POINT('',(-21.,4.,7.));
#10329=CARTESIAN_POINT('',(-21.,0.,-7.));
#10330=CARTESIAN_POINT('Origin',(-20.,-152.5212,-7.));
#10331=CARTESIAN_POINT('Origin',(-20.,4.,-7.));
#10332=CARTESIAN_POINT('Origin',(-20.,4.,-7.));
#10333=CARTESIAN_POINT('Origin',(-20.,4.,-7.));
#10334=CARTESIAN_POINT('Origin',(-20.,4.,-7.));
#10335=CARTESIAN_POINT('Origin',(-75.7512,4.,-7.));
#10336=CARTESIAN_POINT('Origin',(-20.,4.,43.78380184031));
#10337=CARTESIAN_POINT('Origin',(-20.,4.,7.));
#10338=CARTESIAN_POINT('Origin',(-20.,4.,7.));
#10339=CARTESIAN_POINT('Origin',(-20.,4.,7.));
#10340=CARTESIAN_POINT('Origin',(75.7512,4.,7.));
#10341=CARTESIAN_POINT('Origin',(-13.,4.,7.));
#10342=CARTESIAN_POINT('Origin',(-13.,4.,7.));
#10343=CARTESIAN_POINT('Origin',(-21.1,20.,8.));
#10344=CARTESIAN_POINT('',(-12.,20.,7.));
#10345=CARTESIAN_POINT('Origin',(-21.1,20.,7.));
#10346=CARTESIAN_POINT('',(-12.,27.,7.));
#10347=CARTESIAN_POINT('Origin',(-21.1,27.,7.));
#10348=CARTESIAN_POINT('Origin',(-12.,16.4,0.));
#10349=CARTESIAN_POINT('',(-12.,19.4,-3.67394039744206E-16));
#10350=CARTESIAN_POINT('Origin',(-12.,16.4,0.));
#10351=CARTESIAN_POINT('',(-8.,19.4,-3.67394039744206E-16));
#10352=CARTESIAN_POINT('',(-12.,19.4,-3.67394039744206E-16));
#10353=CARTESIAN_POINT('Origin',(-8.,16.4,0.));
#10354=CARTESIAN_POINT('Origin',(-8.,16.4,0.));
#10355=CARTESIAN_POINT('',(-8.,13.775,0.));
#10356=CARTESIAN_POINT('Origin',(-8.,16.4,0.));
#10357=CARTESIAN_POINT('Origin',(12.,16.4,0.));
#10358=CARTESIAN_POINT('',(12.,13.4,-3.67394039744206E-16));
#10359=CARTESIAN_POINT('Origin',(12.,16.4,0.));
#10360=CARTESIAN_POINT('',(8.,13.4,-3.67394039744206E-16));
#10361=CARTESIAN_POINT('',(12.,13.4,-3.67394039744206E-16));
#10362=CARTESIAN_POINT('Origin',(8.,16.4,0.));
#10363=CARTESIAN_POINT('Origin',(8.,16.4,0.));
#10364=CARTESIAN_POINT('',(8.,19.025,0.));
#10365=CARTESIAN_POINT('Origin',(8.,16.4,0.));
#10366=CARTESIAN_POINT('',(0.,0.,0.));
#10367=CARTESIAN_POINT('Origin',(0.,0.,-1.));
#10368=CARTESIAN_POINT('',(-2.309401076759,-4.,-1.));
#10369=CARTESIAN_POINT('',(2.309401076759,-4.,-1.));
#10370=CARTESIAN_POINT('',(-2.309401076759,-4.,-1.));
#10371=CARTESIAN_POINT('',(-4.618802153517,0.,-1.));
#10372=CARTESIAN_POINT('',(-4.618802153517,0.,-1.));
#10373=CARTESIAN_POINT('',(-2.309401076759,4.,-1.));
#10374=CARTESIAN_POINT('',(-2.309401076759,4.,-1.));
#10375=CARTESIAN_POINT('',(2.309401076759,4.,-1.));
#10376=CARTESIAN_POINT('',(2.309401076759,4.,-1.));
#10377=CARTESIAN_POINT('',(4.618802153517,0.,-1.));
#10378=CARTESIAN_POINT('',(4.618802153517,0.,-1.));
#10379=CARTESIAN_POINT('',(2.309401076759,-4.,-1.));
#10380=CARTESIAN_POINT('',(-2.75,0.,-1.));
#10381=CARTESIAN_POINT('Origin',(0.,0.,-1.));
#10382=CARTESIAN_POINT('Origin',(-2.309401076759,-4.,-1.));
#10383=CARTESIAN_POINT('',(2.309401076759,-4.,1.));
#10384=CARTESIAN_POINT('',(2.309401076759,-4.,-1.));
#10385=CARTESIAN_POINT('',(-2.309401076759,-4.,1.));
#10386=CARTESIAN_POINT('',(-2.309401076759,-4.,1.));
#10387=CARTESIAN_POINT('',(-2.309401076759,-4.,-1.));
#10388=CARTESIAN_POINT('Origin',(-4.618802153517,0.,-1.));
#10389=CARTESIAN_POINT('',(-4.618802153517,0.,1.));
#10390=CARTESIAN_POINT('',(-4.618802153517,0.,1.));
#10391=CARTESIAN_POINT('',(-4.618802153517,0.,-1.));
#10392=CARTESIAN_POINT('Origin',(-2.309401076759,4.,-1.));
#10393=CARTESIAN_POINT('',(-2.309401076759,4.,1.));
#10394=CARTESIAN_POINT('',(-2.309401076759,4.,1.));
#10395=CARTESIAN_POINT('',(-2.309401076759,4.,-1.));
#10396=CARTESIAN_POINT('Origin',(2.309401076759,4.,-1.));
#10397=CARTESIAN_POINT('',(2.309401076759,4.,1.));
#10398=CARTESIAN_POINT('',(2.309401076759,4.,1.));
#10399=CARTESIAN_POINT('',(2.309401076759,4.,-1.));
#10400=CARTESIAN_POINT('Origin',(4.618802153517,0.,-1.));
#10401=CARTESIAN_POINT('',(4.618802153517,0.,1.));
#10402=CARTESIAN_POINT('',(4.618802153517,0.,1.));
#10403=CARTESIAN_POINT('',(4.618802153517,0.,-1.));
#10404=CARTESIAN_POINT('Origin',(2.309401076759,-4.,-1.));
#10405=CARTESIAN_POINT('',(2.309401076759,-4.,1.));
#10406=CARTESIAN_POINT('Origin',(0.,0.,1.));
#10407=CARTESIAN_POINT('',(-2.75,-3.36777869765522E-16,1.));
#10408=CARTESIAN_POINT('Origin',(0.,0.,1.));
#10409=CARTESIAN_POINT('Origin',(0.,0.,-5.));
#10410=CARTESIAN_POINT('',(-2.75,0.,-5.));
#10411=CARTESIAN_POINT('',(-2.75,-3.36777869765522E-16,-5.));
#10412=CARTESIAN_POINT('Origin',(0.,0.,-5.));
#10413=CARTESIAN_POINT('Origin',(0.,0.,-5.));
#10414=CARTESIAN_POINT('',(-2.75,-3.36777869765522E-16,6.));
#10415=CARTESIAN_POINT('Origin',(0.,0.,6.));
#10416=CARTESIAN_POINT('',(-2.75,-3.36777869765522E-16,-5.));
#10417=CARTESIAN_POINT('Origin',(0.,0.,-5.));
#10418=CARTESIAN_POINT('',(-1.75,0.,-5.));
#10419=CARTESIAN_POINT('Origin',(0.,0.,-5.));
#10420=CARTESIAN_POINT('Origin',(0.,0.,6.));
#10421=CARTESIAN_POINT('',(-1.75,0.,6.));
#10422=CARTESIAN_POINT('',(-1.75,-2.14313189850787E-16,6.));
#10423=CARTESIAN_POINT('Origin',(0.,0.,6.));
#10424=CARTESIAN_POINT('Origin',(0.,0.,6.));
#10425=CARTESIAN_POINT('Origin',(0.,0.,6.));
#10426=CARTESIAN_POINT('',(-2.475,-3.0310008278897E-16,6.));
#10427=CARTESIAN_POINT('Origin',(0.,0.,6.));
#10428=CARTESIAN_POINT('',(-2.475,-3.0310008278897E-16,1.));
#10429=CARTESIAN_POINT('',(-2.475,-3.0310008278897E-16,6.));
#10430=CARTESIAN_POINT('Origin',(0.,0.,1.));
#10431=CARTESIAN_POINT('Origin',(0.,0.,1.));
#10432=CARTESIAN_POINT('',(2.75,0.,1.));
#10433=CARTESIAN_POINT('Origin',(0.,0.,1.));
#10434=CARTESIAN_POINT('Origin',(0.,0.,-5.));
#10435=CARTESIAN_POINT('',(2.475,-3.0310008278897E-16,-5.));
#10436=CARTESIAN_POINT('Origin',(0.,0.,-5.));
#10437=CARTESIAN_POINT('',(2.475,-3.0310008278897E-16,-1.));
#10438=CARTESIAN_POINT('',(2.475,-3.0310008278897E-16,-5.));
#10439=CARTESIAN_POINT('Origin',(0.,0.,-1.));
#10440=CARTESIAN_POINT('Origin',(0.,0.,-1.));
#10441=CARTESIAN_POINT('',(-2.75,0.,-1.));
#10442=CARTESIAN_POINT('Origin',(0.,0.,-1.));
#10443=CARTESIAN_POINT('',(0.,0.,0.));
#10444=CARTESIAN_POINT('',(0.,6.,0.));
#10445=CARTESIAN_POINT('',(13.,22.4,0.));
#10446=CARTESIAN_POINT('',(-13.,22.4,0.));
#10447=CARTESIAN_POINT('',(0.,0.,0.));
#10448=CARTESIAN_POINT('',(0.,0.,0.));
#10449=CARTESIAN_POINT('Origin',(0.,-9.5,0.));
#10450=CARTESIAN_POINT('',(6.12323399573677E-16,-9.5,-5.));
#10451=CARTESIAN_POINT('Origin',(0.,-9.5,0.));
#10452=CARTESIAN_POINT('',(3.06161699786838E-16,-9.5,-2.5));
#10453=CARTESIAN_POINT('Origin',(0.,-9.5,0.));
#10454=CARTESIAN_POINT('Origin',(0.,5.725,0.));
#10455=CARTESIAN_POINT('',(6.12323399573677E-16,-2.5,-5.));
#10456=CARTESIAN_POINT('',(6.12323399573677E-16,5.725,-5.));
#10457=CARTESIAN_POINT('Origin',(0.,-2.5,0.));
#10458=CARTESIAN_POINT('',(-5.,-7.25,0.));
#10459=CARTESIAN_POINT('',(-5.,-4.75,1.53080849893419E-16));
#10460=CARTESIAN_POINT('Ctrl Pts',(-5.,-7.25,-6.93889390390723E-17));
#10461=CARTESIAN_POINT('Ctrl Pts',(-5.,-7.25,-0.157664715929046));
#10462=CARTESIAN_POINT('Ctrl Pts',(-4.99179575122445,-7.21835421378757,
-0.325388319770619));
#10463=CARTESIAN_POINT('Ctrl Pts',(-4.96215629725421,-7.09057657413409,
-0.633172380752554));
#10464=CARTESIAN_POINT('Ctrl Pts',(-4.94111880834681,-6.99448091912696,
-0.773286033839411));
#10465=CARTESIAN_POINT('Ctrl Pts',(-4.90138825645426,-6.7732705681841,-0.994496384782273));
#10466=CARTESIAN_POINT('Ctrl Pts',(-4.88005597223663,-6.63316335628804,
-1.09057998139517));
#10467=CARTESIAN_POINT('Ctrl Pts',(-4.84973579332106,-6.32540213501313,
-1.21834881761244));
#10468=CARTESIAN_POINT('Ctrl Pts',(-4.84122918275927,-6.15768676334799,
-1.25));
#10469=CARTESIAN_POINT('Ctrl Pts',(-4.84122918275927,-5.84231323665201,
-1.25));
#10470=CARTESIAN_POINT('Ctrl Pts',(-4.84973579332106,-5.67459786498688,
-1.21834881761244));
#10471=CARTESIAN_POINT('Ctrl Pts',(-4.88005597223663,-5.36683664371196,
-1.09057998139517));
#10472=CARTESIAN_POINT('Ctrl Pts',(-4.90138825645426,-5.2267294318159,-0.994496384782273));
#10473=CARTESIAN_POINT('Ctrl Pts',(-4.94111880834681,-5.00551908087304,
-0.773286033839411));
#10474=CARTESIAN_POINT('Ctrl Pts',(-4.96215629725421,-4.90942342586591,
-0.633172380752555));
#10475=CARTESIAN_POINT('Ctrl Pts',(-4.99179575122445,-4.78164578621243,
-0.32538831977062));
#10476=CARTESIAN_POINT('Ctrl Pts',(-5.,-4.75,-0.157664715929046));
#10477=CARTESIAN_POINT('Ctrl Pts',(-5.,-4.75,3.46944695195361E-17));
#10478=CARTESIAN_POINT('Ctrl Pts',(-5.,-4.75,1.38777878078145E-16));
#10479=CARTESIAN_POINT('Ctrl Pts',(-5.,-4.75,0.157664715929046));
#10480=CARTESIAN_POINT('Ctrl Pts',(-4.99179575122445,-4.78164578621243,
0.32538831977062));
#10481=CARTESIAN_POINT('Ctrl Pts',(-4.96215629725421,-4.90942342586591,
0.633172380752555));
#10482=CARTESIAN_POINT('Ctrl Pts',(-4.94111880834681,-5.00551908087304,
0.773286033839411));
#10483=CARTESIAN_POINT('Ctrl Pts',(-4.90138825645426,-5.2267294318159,0.994496384782273));
#10484=CARTESIAN_POINT('Ctrl Pts',(-4.88005597223663,-5.36683664371196,
1.09057998139517));
#10485=CARTESIAN_POINT('Ctrl Pts',(-4.84973579332106,-5.67459786498688,
1.21834881761244));
#10486=CARTESIAN_POINT('Ctrl Pts',(-4.84122918275927,-5.84231323665201,
1.25));
#10487=CARTESIAN_POINT('Ctrl Pts',(-4.84122918275927,-6.,1.25));
#10488=CARTESIAN_POINT('Ctrl Pts',(-4.84122918275927,-6.15768676334799,
1.25));
#10489=CARTESIAN_POINT('Ctrl Pts',(-4.84973579332106,-6.32540213501313,
1.21834881761244));
#10490=CARTESIAN_POINT('Ctrl Pts',(-4.88005597223663,-6.63316335628804,
1.09057998139517));
#10491=CARTESIAN_POINT('Ctrl Pts',(-4.90138825645426,-6.7732705681841,0.994496384782273));
#10492=CARTESIAN_POINT('Ctrl Pts',(-4.94111880834681,-6.99448091912696,
0.773286033839411));
#10493=CARTESIAN_POINT('Ctrl Pts',(-4.96215629725421,-7.09057657413409,
0.633172380752555));
#10494=CARTESIAN_POINT('Ctrl Pts',(-4.99179575122445,-7.21835421378757,
0.32538831977062));
#10495=CARTESIAN_POINT('Ctrl Pts',(-5.,-7.25,0.157664715929046));
#10496=CARTESIAN_POINT('Ctrl Pts',(-5.,-7.25,-3.81639164714898E-16));
#10497=CARTESIAN_POINT('',(5.,-4.75,0.));
#10498=CARTESIAN_POINT('Ctrl Pts',(4.84122918275927,-6.,1.25));
#10499=CARTESIAN_POINT('Ctrl Pts',(4.84122918275927,-5.84231323665201,1.25));
#10500=CARTESIAN_POINT('Ctrl Pts',(4.84973579332106,-5.67459786498687,1.21834881761244));
#10501=CARTESIAN_POINT('Ctrl Pts',(4.88005597223663,-5.36683664371196,1.09057998139517));
#10502=CARTESIAN_POINT('Ctrl Pts',(4.90138825645426,-5.2267294318159,0.994496384782273));
#10503=CARTESIAN_POINT('Ctrl Pts',(4.94111880834681,-5.00551908087304,0.773286033839411));
#10504=CARTESIAN_POINT('Ctrl Pts',(4.96215629725421,-4.90942342586591,0.633172380752555));
#10505=CARTESIAN_POINT('Ctrl Pts',(4.99179575122445,-4.78164578621243,0.32538831977062));
#10506=CARTESIAN_POINT('Ctrl Pts',(5.,-4.75,0.157664715929046));
#10507=CARTESIAN_POINT('Ctrl Pts',(5.,-4.75,-0.157664715929046));
#10508=CARTESIAN_POINT('Ctrl Pts',(4.99179575122445,-4.78164578621243,-0.325388319770619));
#10509=CARTESIAN_POINT('Ctrl Pts',(4.96215629725421,-4.90942342586591,-0.633172380752555));
#10510=CARTESIAN_POINT('Ctrl Pts',(4.94111880834681,-5.00551908087304,-0.773286033839411));
#10511=CARTESIAN_POINT('Ctrl Pts',(4.90138825645426,-5.2267294318159,-0.994496384782273));
#10512=CARTESIAN_POINT('Ctrl Pts',(4.88005597223663,-5.36683664371196,-1.09057998139517));
#10513=CARTESIAN_POINT('Ctrl Pts',(4.84973579332106,-5.67459786498688,-1.21834881761244));
#10514=CARTESIAN_POINT('Ctrl Pts',(4.84122918275927,-5.84231323665201,-1.25));
#10515=CARTESIAN_POINT('Ctrl Pts',(4.84122918275927,-6.15768676334799,-1.25));
#10516=CARTESIAN_POINT('Ctrl Pts',(4.84973579332106,-6.32540213501313,-1.21834881761244));
#10517=CARTESIAN_POINT('Ctrl Pts',(4.88005597223663,-6.63316335628804,-1.09057998139517));
#10518=CARTESIAN_POINT('Ctrl Pts',(4.90138825645426,-6.7732705681841,-0.994496384782273));
#10519=CARTESIAN_POINT('Ctrl Pts',(4.94111880834681,-6.99448091912696,-0.773286033839411));
#10520=CARTESIAN_POINT('Ctrl Pts',(4.96215629725421,-7.09057657413409,-0.633172380752555));
#10521=CARTESIAN_POINT('Ctrl Pts',(4.99179575122445,-7.21835421378757,-0.32538831977062));
#10522=CARTESIAN_POINT('Ctrl Pts',(5.,-7.25,-0.157664715929046));
#10523=CARTESIAN_POINT('Ctrl Pts',(5.,-7.25,0.157664715929046));
#10524=CARTESIAN_POINT('Ctrl Pts',(4.99179575122445,-7.21835421378757,0.325388319770619));
#10525=CARTESIAN_POINT('Ctrl Pts',(4.96215629725421,-7.09057657413409,0.633172380752555));
#10526=CARTESIAN_POINT('Ctrl Pts',(4.94111880834681,-6.99448091912696,0.773286033839411));
#10527=CARTESIAN_POINT('Ctrl Pts',(4.90138825645426,-6.7732705681841,0.994496384782273));
#10528=CARTESIAN_POINT('Ctrl Pts',(4.88005597223663,-6.63316335628804,1.09057998139517));
#10529=CARTESIAN_POINT('Ctrl Pts',(4.84973579332106,-6.32540213501313,1.21834881761244));
#10530=CARTESIAN_POINT('Ctrl Pts',(4.84122918275927,-6.15768676334799,1.25));
#10531=CARTESIAN_POINT('Ctrl Pts',(4.84122918275927,-6.,1.25));
#10532=CARTESIAN_POINT('Origin',(0.,-2.5,0.));
#10533=CARTESIAN_POINT('',(4.28626379701574E-15,-2.5,-35.));
#10534=CARTESIAN_POINT('Origin',(0.,-2.5,0.));
#10535=CARTESIAN_POINT('',(-12.5,-2.5,-20.));
#10536=CARTESIAN_POINT('Origin',(0.,-2.5,-20.));
#10537=CARTESIAN_POINT('',(-12.5,-2.5,20.));
#10538=CARTESIAN_POINT('Origin',(0.,-2.5,20.));
#10539=CARTESIAN_POINT('',(7.5,-2.5,0.));
#10540=CARTESIAN_POINT('Origin',(20.,-2.5,0.));
#10541=CARTESIAN_POINT('',(-32.5,-2.5,0.));
#10542=CARTESIAN_POINT('Origin',(-20.,-2.5,0.));
#10543=CARTESIAN_POINT('',(13.67105307091,-2.5,-19.5));
#10544=CARTESIAN_POINT('Origin',(19.67105307091,-2.5,-19.5));
#10545=CARTESIAN_POINT('',(-25.67105307091,-2.5,-19.5));
#10546=CARTESIAN_POINT('Origin',(-19.67105307091,-2.5,-19.5));
#10547=CARTESIAN_POINT('',(13.67105307091,-2.5,19.5));
#10548=CARTESIAN_POINT('Origin',(19.67105307091,-2.5,19.5));
#10549=CARTESIAN_POINT('',(-25.67105307091,-2.5,19.5));
#10550=CARTESIAN_POINT('Origin',(-19.67105307091,-2.5,19.5));
#10551=CARTESIAN_POINT('Origin',(0.,5.725,0.));
#10552=CARTESIAN_POINT('',(4.28626379701574E-15,-5.,-35.));
#10553=CARTESIAN_POINT('',(4.28626379701574E-15,5.725,-35.));
#10554=CARTESIAN_POINT('Origin',(0.,-5.,0.));
#10555=CARTESIAN_POINT('Origin',(0.,-5.,0.));
#10556=CARTESIAN_POINT('',(4.89858719658941E-15,-5.,-40.));
#10557=CARTESIAN_POINT('Origin',(0.,-5.,0.));
#10558=CARTESIAN_POINT('Origin',(0.,5.725,0.));
#10559=CARTESIAN_POINT('',(4.89858719658941E-15,5.,-40.));
#10560=CARTESIAN_POINT('',(4.89858719658941E-15,5.725,-40.));
#10561=CARTESIAN_POINT('Origin',(0.,5.,0.));
#10562=CARTESIAN_POINT('Origin',(0.,5.,0.));
#10563=CARTESIAN_POINT('',(4.28626379701574E-15,5.,-35.));
#10564=CARTESIAN_POINT('Origin',(0.,5.,0.));
#10565=CARTESIAN_POINT('Origin',(0.,5.725,0.));
#10566=CARTESIAN_POINT('',(4.28626379701574E-15,2.5,-35.));
#10567=CARTESIAN_POINT('',(4.28626379701574E-15,5.725,-35.));
#10568=CARTESIAN_POINT('Origin',(0.,2.5,0.));
#10569=CARTESIAN_POINT('Origin',(0.,2.5,0.));
#10570=CARTESIAN_POINT('',(6.12323399573677E-16,2.5,-5.));
#10571=CARTESIAN_POINT('Origin',(0.,2.5,0.));
#10572=CARTESIAN_POINT('',(-12.5,2.5,-20.));
#10573=CARTESIAN_POINT('Origin',(0.,2.5,-20.));
#10574=CARTESIAN_POINT('',(-12.5,2.5,20.));
#10575=CARTESIAN_POINT('Origin',(0.,2.5,20.));
#10576=CARTESIAN_POINT('',(7.5,2.5,0.));
#10577=CARTESIAN_POINT('Origin',(20.,2.5,0.));
#10578=CARTESIAN_POINT('',(-32.5,2.5,0.));
#10579=CARTESIAN_POINT('Origin',(-20.,2.5,0.));
#10580=CARTESIAN_POINT('',(13.67105307091,2.5,-19.5));
#10581=CARTESIAN_POINT('Origin',(19.67105307091,2.5,-19.5));
#10582=CARTESIAN_POINT('',(-25.67105307091,2.5,-19.5));
#10583=CARTESIAN_POINT('Origin',(-19.67105307091,2.5,-19.5));
#10584=CARTESIAN_POINT('',(13.67105307091,2.5,19.5));
#10585=CARTESIAN_POINT('Origin',(19.67105307091,2.5,19.5));
#10586=CARTESIAN_POINT('',(-25.67105307091,2.5,19.5));
#10587=CARTESIAN_POINT('Origin',(-19.67105307091,2.5,19.5));
#10588=CARTESIAN_POINT('Origin',(0.,5.725,0.));
#10589=CARTESIAN_POINT('',(6.12323399573677E-16,5.,-5.));
#10590=CARTESIAN_POINT('',(6.12323399573677E-16,5.725,-5.));
#10591=CARTESIAN_POINT('Origin',(0.,5.,0.));
#10592=CARTESIAN_POINT('Origin',(0.,5.,0.));
#10593=CARTESIAN_POINT('',(3.06161699786838E-16,5.,-2.5));
#10594=CARTESIAN_POINT('Origin',(0.,5.,0.));
#10595=CARTESIAN_POINT('Origin',(0.,5.725,0.));
#10596=CARTESIAN_POINT('',(3.06161699786838E-16,5.725,-2.5));
#10597=CARTESIAN_POINT('',(-2.5,-4.75,0.));
#10598=CARTESIAN_POINT('Ctrl Pts',(-2.1650635094611,-6.,1.25));
#10599=CARTESIAN_POINT('Ctrl Pts',(-2.1650635094611,-5.83961866629939,1.25));
#10600=CARTESIAN_POINT('Ctrl Pts',(-2.18478179494117,-5.67107674842089,
1.21735698059595));
#10601=CARTESIAN_POINT('Ctrl Pts',(-2.25149501557585,-5.36427205061522,
1.08903588717028));
#10602=CARTESIAN_POINT('Ctrl Pts',(-2.29712558443605,-5.22567783219742,
0.993444785163793));
#10603=CARTESIAN_POINT('Ctrl Pts',(-2.37983326258812,-5.00685388429146,
0.774620837257829));
#10604=CARTESIAN_POINT('Ctrl Pts',(-2.42283105129935,-4.91104365009427,
0.635925947642968));
#10605=CARTESIAN_POINT('Ctrl Pts',(-2.48323996043832,-4.78254511766359,
0.328681344361069));
#10606=CARTESIAN_POINT('Ctrl Pts',(-2.5,-4.75,0.159944126385861));
#10607=CARTESIAN_POINT('Ctrl Pts',(-2.5,-4.75,-0.159944126385861));
#10608=CARTESIAN_POINT('Ctrl Pts',(-2.48323996043832,-4.78254511766359,
-0.328681344361069));
#10609=CARTESIAN_POINT('Ctrl Pts',(-2.42283105129935,-4.91104365009427,
-0.635925947642968));
#10610=CARTESIAN_POINT('Ctrl Pts',(-2.37983326258812,-5.00685388429146,
-0.774620837257828));
#10611=CARTESIAN_POINT('Ctrl Pts',(-2.29712558443605,-5.22567783219742,
-0.993444785163793));
#10612=CARTESIAN_POINT('Ctrl Pts',(-2.25149501557585,-5.36427205061522,
-1.08903588717028));
#10613=CARTESIAN_POINT('Ctrl Pts',(-2.18478179494117,-5.67107674842089,
-1.21735698059595));
#10614=CARTESIAN_POINT('Ctrl Pts',(-2.1650635094611,-5.83961866629939,-1.25));
#10615=CARTESIAN_POINT('Ctrl Pts',(-2.1650635094611,-6.16038133370061,-1.25));
#10616=CARTESIAN_POINT('Ctrl Pts',(-2.18478179494117,-6.32892325157911,
-1.21735698059595));
#10617=CARTESIAN_POINT('Ctrl Pts',(-2.25149501557585,-6.63572794938478,
-1.08903588717028));
#10618=CARTESIAN_POINT('Ctrl Pts',(-2.29712558443605,-6.77432216780258,
-0.993444785163793));
#10619=CARTESIAN_POINT('Ctrl Pts',(-2.37983326258812,-6.99314611570854,
-0.774620837257829));
#10620=CARTESIAN_POINT('Ctrl Pts',(-2.42283105129935,-7.08895634990573,
-0.635925947642969));
#10621=CARTESIAN_POINT('Ctrl Pts',(-2.48323996043832,-7.21745488233641,
-0.32868134436107));
#10622=CARTESIAN_POINT('Ctrl Pts',(-2.5,-7.25,-0.159944126385861));
#10623=CARTESIAN_POINT('Ctrl Pts',(-2.5,-7.25,0.159944126385861));
#10624=CARTESIAN_POINT('Ctrl Pts',(-2.48323996043832,-7.21745488233641,
0.328681344361069));
#10625=CARTESIAN_POINT('Ctrl Pts',(-2.42283105129935,-7.08895634990573,
0.635925947642968));
#10626=CARTESIAN_POINT('Ctrl Pts',(-2.37983326258812,-6.99314611570854,
0.774620837257828));
#10627=CARTESIAN_POINT('Ctrl Pts',(-2.29712558443605,-6.77432216780258,
0.993444785163793));
#10628=CARTESIAN_POINT('Ctrl Pts',(-2.25149501557585,-6.63572794938478,
1.08903588717028));
#10629=CARTESIAN_POINT('Ctrl Pts',(-2.18478179494117,-6.32892325157911,
1.21735698059595));
#10630=CARTESIAN_POINT('Ctrl Pts',(-2.1650635094611,-6.16038133370061,1.25));
#10631=CARTESIAN_POINT('Ctrl Pts',(-2.1650635094611,-6.,1.25));
#10632=CARTESIAN_POINT('',(2.5,-7.25,0.));
#10633=CARTESIAN_POINT('',(2.5,-4.75,1.45929363985782E-16));
#10634=CARTESIAN_POINT('Ctrl Pts',(2.5,-7.25,-2.77555756156289E-16));
#10635=CARTESIAN_POINT('Ctrl Pts',(2.5,-7.25,-0.159944126385861));
#10636=CARTESIAN_POINT('Ctrl Pts',(2.48323996043832,-7.21745488233641,-0.328681344361069));
#10637=CARTESIAN_POINT('Ctrl Pts',(2.42283105129935,-7.08895634990573,-0.635925947642968));
#10638=CARTESIAN_POINT('Ctrl Pts',(2.37983326258812,-6.99314611570854,-0.774620837257829));
#10639=CARTESIAN_POINT('Ctrl Pts',(2.29712558443605,-6.77432216780258,-0.993444785163793));
#10640=CARTESIAN_POINT('Ctrl Pts',(2.25149501557585,-6.63572794938478,-1.08903588717028));
#10641=CARTESIAN_POINT('Ctrl Pts',(2.18478179494117,-6.32892325157911,-1.21735698059595));
#10642=CARTESIAN_POINT('Ctrl Pts',(2.1650635094611,-6.16038133370061,-1.25));
#10643=CARTESIAN_POINT('Ctrl Pts',(2.1650635094611,-5.83961866629939,-1.25));
#10644=CARTESIAN_POINT('Ctrl Pts',(2.18478179494117,-5.67107674842089,-1.21735698059595));
#10645=CARTESIAN_POINT('Ctrl Pts',(2.25149501557585,-5.36427205061522,-1.08903588717028));
#10646=CARTESIAN_POINT('Ctrl Pts',(2.29712558443605,-5.22567783219742,-0.993444785163793));
#10647=CARTESIAN_POINT('Ctrl Pts',(2.37983326258812,-5.00685388429146,-0.774620837257828));
#10648=CARTESIAN_POINT('Ctrl Pts',(2.42283105129935,-4.91104365009427,-0.635925947642968));
#10649=CARTESIAN_POINT('Ctrl Pts',(2.48323996043832,-4.78254511766359,-0.328681344361069));
#10650=CARTESIAN_POINT('Ctrl Pts',(2.5,-4.75,-0.159944126385861));
#10651=CARTESIAN_POINT('Ctrl Pts',(2.5,-4.75,2.42861286636753E-16));
#10652=CARTESIAN_POINT('Ctrl Pts',(2.5,-4.75,1.38777878078145E-16));
#10653=CARTESIAN_POINT('Ctrl Pts',(2.5,-4.75,0.159944126385861));
#10654=CARTESIAN_POINT('Ctrl Pts',(2.48323996043832,-4.78254511766359,0.328681344361069));
#10655=CARTESIAN_POINT('Ctrl Pts',(2.42283105129935,-4.91104365009427,0.635925947642968));
#10656=CARTESIAN_POINT('Ctrl Pts',(2.37983326258812,-5.00685388429146,0.774620837257829));
#10657=CARTESIAN_POINT('Ctrl Pts',(2.29712558443605,-5.22567783219742,0.993444785163793));
#10658=CARTESIAN_POINT('Ctrl Pts',(2.25149501557585,-5.36427205061522,1.08903588717028));
#10659=CARTESIAN_POINT('Ctrl Pts',(2.18478179494117,-5.67107674842089,1.21735698059595));
#10660=CARTESIAN_POINT('Ctrl Pts',(2.1650635094611,-5.83961866629939,1.25));
#10661=CARTESIAN_POINT('Ctrl Pts',(2.1650635094611,-6.,1.25));
#10662=CARTESIAN_POINT('Ctrl Pts',(2.1650635094611,-6.16038133370061,1.25));
#10663=CARTESIAN_POINT('Ctrl Pts',(2.18478179494117,-6.32892325157911,1.21735698059595));
#10664=CARTESIAN_POINT('Ctrl Pts',(2.25149501557585,-6.63572794938478,1.08903588717028));
#10665=CARTESIAN_POINT('Ctrl Pts',(2.29712558443605,-6.77432216780258,0.993444785163793));
#10666=CARTESIAN_POINT('Ctrl Pts',(2.37983326258812,-6.99314611570854,0.774620837257828));
#10667=CARTESIAN_POINT('Ctrl Pts',(2.42283105129935,-7.08895634990573,0.635925947642969));
#10668=CARTESIAN_POINT('Ctrl Pts',(2.48323996043832,-7.21745488233641,0.328681344361069));
#10669=CARTESIAN_POINT('Ctrl Pts',(2.5,-7.25,0.159944126385861));
#10670=CARTESIAN_POINT('Ctrl Pts',(2.5,-7.25,-3.46944695195361E-16));
#10671=CARTESIAN_POINT('Origin',(-8.8,-6.,0.));
#10672=CARTESIAN_POINT('',(-8.8,-4.75,1.53080849893419E-16));
#10673=CARTESIAN_POINT('Origin',(-8.8,-6.,0.));
#10674=CARTESIAN_POINT('',(-8.8,-4.75,1.53080849893419E-16));
#10675=CARTESIAN_POINT('Origin',(0.,-11.6,-20.));
#10676=CARTESIAN_POINT('',(-12.5,-11.6,-20.));
#10677=CARTESIAN_POINT('Origin',(0.,-11.6,20.));
#10678=CARTESIAN_POINT('',(-12.5,-11.6,20.));
#10679=CARTESIAN_POINT('Origin',(20.,-11.6,0.));
#10680=CARTESIAN_POINT('',(7.5,-11.6,1.53080849893419E-15));
#10681=CARTESIAN_POINT('Origin',(-20.,-11.6,0.));
#10682=CARTESIAN_POINT('',(-32.5,-11.6,1.53080849893419E-15));
#10683=CARTESIAN_POINT('Origin',(19.67105307091,-11.6,-19.5));
#10684=CARTESIAN_POINT('',(13.67105307091,-11.6,-19.5));
#10685=CARTESIAN_POINT('Origin',(-19.67105307091,-11.6,-19.5));
#10686=CARTESIAN_POINT('',(-25.67105307091,-11.6,-19.5));
#10687=CARTESIAN_POINT('Origin',(19.67105307091,-11.6,19.5));
#10688=CARTESIAN_POINT('',(13.67105307091,-11.6,19.5));
#10689=CARTESIAN_POINT('Origin',(-19.67105307091,-11.6,19.5));
#10690=CARTESIAN_POINT('',(-25.67105307091,-11.6,19.5));
#10691=CARTESIAN_POINT('',(0.,0.,0.));
#10692=CARTESIAN_POINT('',(0.,0.,0.));
#10693=CARTESIAN_POINT('Origin',(0.,18.,2.));
#10694=CARTESIAN_POINT('',(-6.,18.,5.));
#10695=CARTESIAN_POINT('Origin',(0.,18.,5.));
#10696=CARTESIAN_POINT('',(-6.,18.,3.75));
#10697=CARTESIAN_POINT('',(-6.,18.,2.));
#10698=CARTESIAN_POINT('',(-5.868347297153,16.75,2.5));
#10699=CARTESIAN_POINT('Ctrl Pts',(-5.86834729715275,16.75,2.5));
#10700=CARTESIAN_POINT('Ctrl Pts',(-5.86834729715275,16.75,2.65745525063995));
#10701=CARTESIAN_POINT('Ctrl Pts',(-5.87534197873269,16.7815621590215,2.82507913768158));
#10702=CARTESIAN_POINT('Ctrl Pts',(-5.90038488226116,16.9092698316582,3.13290995658393));
#10703=CARTESIAN_POINT('Ctrl Pts',(-5.91804743154611,17.0053912037911,3.27315815675743));
#10704=CARTESIAN_POINT('Ctrl Pts',(-5.9510289473619,17.2268345143215,3.49460146728784));
#10705=CARTESIAN_POINT('Ctrl Pts',(-5.96852269967858,17.3670858177603,3.59072857638709));
#10706=CARTESIAN_POINT('Ctrl Pts',(-5.99317707212167,17.6749274551324,3.71844041497889));
#10707=CARTESIAN_POINT('Ctrl Pts',(-6.,17.8425551713404,3.75));
#10708=CARTESIAN_POINT('Ctrl Pts',(-6.,18.,3.75));
#10709=CARTESIAN_POINT('',(5.868347297153,16.75,2.5));
#10710=CARTESIAN_POINT('Origin',(0.,18.,2.5));
#10711=CARTESIAN_POINT('',(6.,18.,3.75));
#10712=CARTESIAN_POINT('Ctrl Pts',(6.,18.,3.75));
#10713=CARTESIAN_POINT('Ctrl Pts',(6.,17.8425551713404,3.75));
#10714=CARTESIAN_POINT('Ctrl Pts',(5.99317707212168,17.6749274551324,3.71844041497889));
#10715=CARTESIAN_POINT('Ctrl Pts',(5.96852269967858,17.3670858177603,3.59072857638709));
#10716=CARTESIAN_POINT('Ctrl Pts',(5.9510289473619,17.2268345143215,3.49460146728784));
#10717=CARTESIAN_POINT('Ctrl Pts',(5.91804743154611,17.0053912037911,3.27315815675743));
#10718=CARTESIAN_POINT('Ctrl Pts',(5.90038488226116,16.9092698316582,3.13290995658393));
#10719=CARTESIAN_POINT('Ctrl Pts',(5.87534197873269,16.7815621590215,2.82507913768158));
#10720=CARTESIAN_POINT('Ctrl Pts',(5.86834729715275,16.75,2.65745525063995));
#10721=CARTESIAN_POINT('Ctrl Pts',(5.86834729715275,16.75,2.5));
#10722=CARTESIAN_POINT('',(5.941847823325,17.16666666667,1.568305009375));
#10723=CARTESIAN_POINT('Ctrl Pts',(5.94184782332521,17.166666666666,1.56830500937566));
#10724=CARTESIAN_POINT('Ctrl Pts',(5.95606809991403,17.2680603300616,1.47761575983942));
#10725=CARTESIAN_POINT('Ctrl Pts',(5.97033187405027,17.3896756931327,1.39989973971076));
#10726=CARTESIAN_POINT('Ctrl Pts',(5.99317707212167,17.6749274551324,1.28155958502111));
#10727=CARTESIAN_POINT('Ctrl Pts',(6.,17.8425551713404,1.25));
#10728=CARTESIAN_POINT('Ctrl Pts',(6.,18.1574448286596,1.25));
#10729=CARTESIAN_POINT('Ctrl Pts',(5.99317707212167,18.3250725448676,1.28155958502111));
#10730=CARTESIAN_POINT('Ctrl Pts',(5.96852269967858,18.6329141822397,1.40927142361291));
#10731=CARTESIAN_POINT('Ctrl Pts',(5.9510289473619,18.7731654856785,1.50539853271216));
#10732=CARTESIAN_POINT('Ctrl Pts',(5.91804743154611,18.9946087962089,1.72684184324257));
#10733=CARTESIAN_POINT('Ctrl Pts',(5.90038488226116,19.0907301683418,1.86709004341607));
#10734=CARTESIAN_POINT('Ctrl Pts',(5.87534197873269,19.2184378409785,2.17492086231842));
#10735=CARTESIAN_POINT('Ctrl Pts',(5.86834729715275,19.25,2.34254474936005));
#10736=CARTESIAN_POINT('Ctrl Pts',(5.86834729715275,19.25,2.5));
#10737=CARTESIAN_POINT('Ctrl Pts',(5.86834729715275,19.25,2.65745525063995));
#10738=CARTESIAN_POINT('Ctrl Pts',(5.87534197873269,19.2184378409785,2.82507913768158));
#10739=CARTESIAN_POINT('Ctrl Pts',(5.90038488226116,19.0907301683418,3.13290995658393));
#10740=CARTESIAN_POINT('Ctrl Pts',(5.91804743154611,18.9946087962089,3.27315815675743));
#10741=CARTESIAN_POINT('Ctrl Pts',(5.9510289473619,18.7731654856785,3.49460146728784));
#10742=CARTESIAN_POINT('Ctrl Pts',(5.96852269967858,18.6329141822397,3.59072857638709));
#10743=CARTESIAN_POINT('Ctrl Pts',(5.99317707212167,18.3250725448676,3.71844041497889));
#10744=CARTESIAN_POINT('Ctrl Pts',(6.,18.1574448286596,3.75));
#10745=CARTESIAN_POINT('Ctrl Pts',(6.,18.,3.75));
#10746=CARTESIAN_POINT('',(5.94184782373737,17.1666666696037,-1.7));
#10747=CARTESIAN_POINT('',(5.941847824424,17.1666666745,-1.7));
#10748=CARTESIAN_POINT('',(-6.,18.,-1.7));
#10749=CARTESIAN_POINT('Origin',(0.,18.,-1.7));
#10750=CARTESIAN_POINT('',(-6.,18.,1.25));
#10751=CARTESIAN_POINT('',(-6.,18.,2.));
#10752=CARTESIAN_POINT('Ctrl Pts',(-6.,18.,3.75));
#10753=CARTESIAN_POINT('Ctrl Pts',(-6.,18.1574448286596,3.75));
#10754=CARTESIAN_POINT('Ctrl Pts',(-5.99317707212167,18.3250725448676,3.71844041497889));
#10755=CARTESIAN_POINT('Ctrl Pts',(-5.96852269967858,18.6329141822397,3.59072857638709));
#10756=CARTESIAN_POINT('Ctrl Pts',(-5.9510289473619,18.7731654856785,3.49460146728784));
#10757=CARTESIAN_POINT('Ctrl Pts',(-5.91804743154611,18.9946087962089,3.27315815675743));
#10758=CARTESIAN_POINT('Ctrl Pts',(-5.90038488226116,19.0907301683418,3.13290995658393));
#10759=CARTESIAN_POINT('Ctrl Pts',(-5.87534197873269,19.2184378409785,2.82507913768158));
#10760=CARTESIAN_POINT('Ctrl Pts',(-5.86834729715275,19.25,2.65745525063995));
#10761=CARTESIAN_POINT('Ctrl Pts',(-5.86834729715275,19.25,2.5));
#10762=CARTESIAN_POINT('Ctrl Pts',(-5.86834729715275,19.25,2.34254474936005));
#10763=CARTESIAN_POINT('Ctrl Pts',(-5.87534197873269,19.2184378409785,2.17492086231842));
#10764=CARTESIAN_POINT('Ctrl Pts',(-5.90038488226116,19.0907301683418,1.86709004341607));
#10765=CARTESIAN_POINT('Ctrl Pts',(-5.91804743154611,18.9946087962089,1.72684184324257));
#10766=CARTESIAN_POINT('Ctrl Pts',(-5.9510289473619,18.7731654856785,1.50539853271216));
#10767=CARTESIAN_POINT('Ctrl Pts',(-5.96852269967858,18.6329141822397,1.40927142361291));
#10768=CARTESIAN_POINT('Ctrl Pts',(-5.99317707212167,18.3250725448676,1.28155958502111));
#10769=CARTESIAN_POINT('Ctrl Pts',(-6.,18.1574448286596,1.25));
#10770=CARTESIAN_POINT('Ctrl Pts',(-6.,18.,1.25));
#10771=CARTESIAN_POINT('Origin',(0.,0.,-2.));
#10772=CARTESIAN_POINT('',(-5.644755432159,17.20833333333,-2.));
#10773=CARTESIAN_POINT('',(5.644755432159,17.20833333333,-2.));
#10774=CARTESIAN_POINT('Origin',(0.,18.,-2.));
#10775=CARTESIAN_POINT('',(3.168985505772,-0.4444444444442,-2.));
#10776=CARTESIAN_POINT('',(5.644755432159,17.20833333333,-2.));
#10777=CARTESIAN_POINT('',(-3.168985505773,-0.4444444444444,-2.));
#10778=CARTESIAN_POINT('Origin',(0.,0.,-2.));
#10779=CARTESIAN_POINT('',(-3.168985505773,-0.4444444444444,-2.));
#10780=CARTESIAN_POINT('',(-2.5,18.,-2.));
#10781=CARTESIAN_POINT('Origin',(0.,18.,-2.));
#10782=CARTESIAN_POINT('',(-1.25,-1.53080849893419E-16,-2.));
#10783=CARTESIAN_POINT('Origin',(0.,0.,-2.));
#10784=CARTESIAN_POINT('Origin',(0.,0.,-2.));
#10785=CARTESIAN_POINT('',(-1.25,-1.53080849893419E-16,2.));
#10786=CARTESIAN_POINT('',(-1.25,-1.53080849893419E-16,-2.));
#10787=CARTESIAN_POINT('Origin',(0.,0.,2.));
#10788=CARTESIAN_POINT('Origin',(0.,0.,2.));
#10789=CARTESIAN_POINT('',(-5.594625601103,14.69089674028,2.));
#10790=CARTESIAN_POINT('',(5.594625601103,14.69089674028,2.));
#10791=CARTESIAN_POINT('Origin',(0.,18.,2.));
#10792=CARTESIAN_POINT('',(-3.46607789694,-0.4861111111111,2.));
#10793=CARTESIAN_POINT('',(-5.594625601103,14.69089674028,2.));
#10794=CARTESIAN_POINT('',(3.46607789694,-0.4861111111111,2.));
#10795=CARTESIAN_POINT('Origin',(0.,0.,2.));
#10796=CARTESIAN_POINT('',(3.46607789694,-0.4861111111111,2.));
#10797=CARTESIAN_POINT('Origin',(0.,18.,2.5));
#10798=CARTESIAN_POINT('',(5.884205625306,16.75566526407,2.38112584404));
#10799=CARTESIAN_POINT('Ctrl Pts',(5.88420562530688,16.7556652640704,2.38112584403824));
#10800=CARTESIAN_POINT('Ctrl Pts',(5.79043247403846,16.0870423103697,2.19077963448577));
#10801=CARTESIAN_POINT('Ctrl Pts',(5.68686691397717,15.3485973532238,2.));
#10802=CARTESIAN_POINT('Ctrl Pts',(5.59462560110366,14.6908967402821,2.));
#10803=CARTESIAN_POINT('Ctrl Pts',(5.86834729715275,16.75,2.5));
#10804=CARTESIAN_POINT('Ctrl Pts',(5.86834729715275,16.75,2.48193013436365));
#10805=CARTESIAN_POINT('Ctrl Pts',(5.86943196932979,16.7503925868786,2.46381885206853));
#10806=CARTESIAN_POINT('Ctrl Pts',(5.87426960134035,16.7521318837435,2.42379416578773));
#10807=CARTESIAN_POINT('Ctrl Pts',(5.87850100129599,16.7536496858429,2.40222423989646));
#10808=CARTESIAN_POINT('Ctrl Pts',(5.88420562530614,16.7556652640689,2.38112584403993));
#10809=CARTESIAN_POINT('',(-5.884205625306,16.75566526407,2.38112584404));
#10810=CARTESIAN_POINT('Ctrl Pts',(-5.88420562530614,16.7556652640689,2.38112584403993));
#10811=CARTESIAN_POINT('Ctrl Pts',(-5.88352496284375,16.7554247699651,2.38364325553814));
#10812=CARTESIAN_POINT('Ctrl Pts',(-5.88286503903123,16.7551912573634,2.38616828635534));
#10813=CARTESIAN_POINT('Ctrl Pts',(-5.87300883084945,16.7516991206043,2.42523264769952));
#10814=CARTESIAN_POINT('Ctrl Pts',(-5.86834729715275,16.75,2.46252726842572));
#10815=CARTESIAN_POINT('Ctrl Pts',(-5.86834729715275,16.75,2.5));
#10816=CARTESIAN_POINT('Ctrl Pts',(-5.59462560110203,14.6908967402794,2.));
#10817=CARTESIAN_POINT('Ctrl Pts',(-5.68686691397567,15.348597353222,2.00000000000015));
#10818=CARTESIAN_POINT('Ctrl Pts',(-5.79043247403725,16.0870423103699,2.19077963448226));
#10819=CARTESIAN_POINT('Ctrl Pts',(-5.88420562530548,16.7556652640693,2.3811258440429));
#10820=CARTESIAN_POINT('Origin',(-5.941847823325,17.16666666667,-2.));
#10821=CARTESIAN_POINT('',(-3.46607789546553,-0.48611112162235,-1.7));
#10822=CARTESIAN_POINT('',(-5.94184782319004,17.1666666657008,-1.7));
#10823=CARTESIAN_POINT('',(-3.466077893795,-0.4861111335351,-1.7));
#10824=CARTESIAN_POINT('',(-3.466077893795,-0.4861111335351,-1.7));
#10825=CARTESIAN_POINT('',(-5.941847823325,17.16666666667,1.568305009375));
#10826=CARTESIAN_POINT('Origin',(-6.05872130529396,18.,2.5));
#10827=CARTESIAN_POINT('',(-5.941847822783,17.1666666628,-1.7));
#10828=CARTESIAN_POINT('Origin',(-3.13864717244,-0.6607633563004,-1.7));
#10829=CARTESIAN_POINT('Origin',(-3.168985505773,-0.4444444444444,-1.7));
#10830=CARTESIAN_POINT('Origin',(-5.644755432159,17.20833333333,-1.7));
#10831=CARTESIAN_POINT('Origin',(0.,18.,-1.7));
#10832=CARTESIAN_POINT('Origin',(0.,18.,-1.7));
#10833=CARTESIAN_POINT('Origin',(5.644755432159,17.20833333333,-1.7));
#10834=CARTESIAN_POINT('Origin',(5.675093765492,17.42465224519,-1.7));
#10835=CARTESIAN_POINT('',(3.46607789817656,-0.486111102291924,-1.7));
#10836=CARTESIAN_POINT('',(5.941847824424,17.1666666745,-1.7));
#10837=CARTESIAN_POINT('Origin',(3.168985505773,-0.4444444444444,-1.7));
#10838=CARTESIAN_POINT('Origin',(0.,0.,-1.7));
#10839=CARTESIAN_POINT('Origin',(0.,0.,-1.7));
#10840=CARTESIAN_POINT('Origin',(0.,0.,-2.));
#10841=CARTESIAN_POINT('',(3.466077899139,-0.4861110954326,-1.7));
#10842=CARTESIAN_POINT('Origin',(3.46607789694,-0.4861111111111,-2.));
#10843=CARTESIAN_POINT('Origin',(6.05872130529521,18.,2.5));
#10844=CARTESIAN_POINT('Origin',(-7.75,18.,2.5));
#10845=CARTESIAN_POINT('Ctrl Pts',(-6.,18.,1.25));
#10846=CARTESIAN_POINT('Ctrl Pts',(-6.,17.8425551713404,1.25));
#10847=CARTESIAN_POINT('Ctrl Pts',(-5.99317707212167,17.6749274551324,1.28155958502111));
#10848=CARTESIAN_POINT('Ctrl Pts',(-5.97033187405036,17.3896756931338,1.39989973971032));
#10849=CARTESIAN_POINT('Ctrl Pts',(-5.95606809991427,17.2680603300636,1.47761575983813));
#10850=CARTESIAN_POINT('Ctrl Pts',(-5.94184782332556,17.1666666666685,1.56830500937343));
#10851=CARTESIAN_POINT('',(-2.5,18.,3.75));
#10852=CARTESIAN_POINT('',(-7.75,18.,3.75));
#10853=CARTESIAN_POINT('',(-2.5,18.,1.25));
#10854=CARTESIAN_POINT('Ctrl Pts',(-2.5,18.,1.25));
#10855=CARTESIAN_POINT('Ctrl Pts',(-2.5,17.8400558736141,1.25));
#10856=CARTESIAN_POINT('Ctrl Pts',(-2.48323996043832,17.6713186556389,1.28254511766359));
#10857=CARTESIAN_POINT('Ctrl Pts',(-2.42283105129935,17.364074052357,1.41104365009428));
#10858=CARTESIAN_POINT('Ctrl Pts',(-2.37983326258812,17.2253791627422,1.50685388429146));
#10859=CARTESIAN_POINT('Ctrl Pts',(-2.29712558443605,17.0065552148362,1.72567783219742));
#10860=CARTESIAN_POINT('Ctrl Pts',(-2.25149501557585,16.9109641128297,1.86427205061522));
#10861=CARTESIAN_POINT('Ctrl Pts',(-2.18478179494117,16.7826430194041,2.17107674842089));
#10862=CARTESIAN_POINT('Ctrl Pts',(-2.1650635094611,16.75,2.33961866629939));
#10863=CARTESIAN_POINT('Ctrl Pts',(-2.1650635094611,16.75,2.66038133370061));
#10864=CARTESIAN_POINT('Ctrl Pts',(-2.18478179494117,16.7826430194041,2.82892325157911));
#10865=CARTESIAN_POINT('Ctrl Pts',(-2.25149501557585,16.9109641128297,3.13572794938478));
#10866=CARTESIAN_POINT('Ctrl Pts',(-2.29712558443605,17.0065552148362,3.27432216780258));
#10867=CARTESIAN_POINT('Ctrl Pts',(-2.37983326258812,17.2253791627422,3.49314611570854));
#10868=CARTESIAN_POINT('Ctrl Pts',(-2.42283105129935,17.364074052357,3.58895634990573));
#10869=CARTESIAN_POINT('Ctrl Pts',(-2.48323996043832,17.6713186556389,3.71745488233641));
#10870=CARTESIAN_POINT('Ctrl Pts',(-2.5,17.8400558736141,3.75));
#10871=CARTESIAN_POINT('Ctrl Pts',(-2.5,18.,3.75));
#10872=CARTESIAN_POINT('Ctrl Pts',(-2.5,18.,3.75));
#10873=CARTESIAN_POINT('Ctrl Pts',(-2.5,18.1599441263859,3.75));
#10874=CARTESIAN_POINT('Ctrl Pts',(-2.48323996043832,18.3286813443611,3.71745488233641));
#10875=CARTESIAN_POINT('Ctrl Pts',(-2.42283105129935,18.635925947643,3.58895634990573));
#10876=CARTESIAN_POINT('Ctrl Pts',(-2.37983326258812,18.7746208372578,3.49314611570854));
#10877=CARTESIAN_POINT('Ctrl Pts',(-2.29712558443605,18.9934447851638,3.27432216780258));
#10878=CARTESIAN_POINT('Ctrl Pts',(-2.25149501557585,19.0890358871703,3.13572794938478));
#10879=CARTESIAN_POINT('Ctrl Pts',(-2.18478179494117,19.2173569805959,2.82892325157911));
#10880=CARTESIAN_POINT('Ctrl Pts',(-2.1650635094611,19.25,2.66038133370061));
#10881=CARTESIAN_POINT('Ctrl Pts',(-2.1650635094611,19.25,2.5));
#10882=CARTESIAN_POINT('Ctrl Pts',(-2.1650635094611,19.25,2.33961866629939));
#10883=CARTESIAN_POINT('Ctrl Pts',(-2.18478179494117,19.2173569805959,2.17107674842089));
#10884=CARTESIAN_POINT('Ctrl Pts',(-2.25149501557585,19.0890358871703,1.86427205061522));
#10885=CARTESIAN_POINT('Ctrl Pts',(-2.29712558443605,18.9934447851638,1.72567783219742));
#10886=CARTESIAN_POINT('Ctrl Pts',(-2.37983326258812,18.7746208372578,1.50685388429146));
#10887=CARTESIAN_POINT('Ctrl Pts',(-2.42283105129935,18.635925947643,1.41104365009428));
#10888=CARTESIAN_POINT('Ctrl Pts',(-2.48323996043832,18.3286813443611,1.28254511766359));
#10889=CARTESIAN_POINT('Ctrl Pts',(-2.5,18.1599441263859,1.25));
#10890=CARTESIAN_POINT('Ctrl Pts',(-2.5,18.,1.25));
#10891=CARTESIAN_POINT('Origin',(-7.75,18.,2.5));
#10892=CARTESIAN_POINT('',(2.5,18.,1.25));
#10893=CARTESIAN_POINT('',(2.5,18.,3.75));
#10894=CARTESIAN_POINT('Ctrl Pts',(2.5,18.,1.25));
#10895=CARTESIAN_POINT('Ctrl Pts',(2.5,18.1599441263859,1.25));
#10896=CARTESIAN_POINT('Ctrl Pts',(2.48323996043832,18.3286813443611,1.28254511766359));
#10897=CARTESIAN_POINT('Ctrl Pts',(2.42283105129935,18.635925947643,1.41104365009428));
#10898=CARTESIAN_POINT('Ctrl Pts',(2.37983326258812,18.7746208372578,1.50685388429146));
#10899=CARTESIAN_POINT('Ctrl Pts',(2.29712558443605,18.9934447851638,1.72567783219742));
#10900=CARTESIAN_POINT('Ctrl Pts',(2.25149501557585,19.0890358871703,1.86427205061522));
#10901=CARTESIAN_POINT('Ctrl Pts',(2.18478179494117,19.2173569805959,2.17107674842089));
#10902=CARTESIAN_POINT('Ctrl Pts',(2.1650635094611,19.25,2.33961866629939));
#10903=CARTESIAN_POINT('Ctrl Pts',(2.1650635094611,19.25,2.5));
#10904=CARTESIAN_POINT('Ctrl Pts',(2.1650635094611,19.25,2.66038133370061));
#10905=CARTESIAN_POINT('Ctrl Pts',(2.18478179494117,19.2173569805959,2.82892325157911));
#10906=CARTESIAN_POINT('Ctrl Pts',(2.25149501557585,19.0890358871703,3.13572794938478));
#10907=CARTESIAN_POINT('Ctrl Pts',(2.29712558443605,18.9934447851638,3.27432216780258));
#10908=CARTESIAN_POINT('Ctrl Pts',(2.37983326258812,18.7746208372578,3.49314611570854));
#10909=CARTESIAN_POINT('Ctrl Pts',(2.42283105129935,18.635925947643,3.58895634990573));
#10910=CARTESIAN_POINT('Ctrl Pts',(2.48323996043832,18.3286813443611,3.71745488233641));
#10911=CARTESIAN_POINT('Ctrl Pts',(2.5,18.1599441263859,3.75));
#10912=CARTESIAN_POINT('Ctrl Pts',(2.5,18.,3.75));
#10913=CARTESIAN_POINT('Ctrl Pts',(2.5,18.,3.75));
#10914=CARTESIAN_POINT('Ctrl Pts',(2.5,17.8400558736141,3.75));
#10915=CARTESIAN_POINT('Ctrl Pts',(2.48323996043832,17.6713186556389,3.71745488233641));
#10916=CARTESIAN_POINT('Ctrl Pts',(2.42283105129935,17.364074052357,3.58895634990573));
#10917=CARTESIAN_POINT('Ctrl Pts',(2.37983326258812,17.2253791627422,3.49314611570854));
#10918=CARTESIAN_POINT('Ctrl Pts',(2.29712558443605,17.0065552148362,3.27432216780258));
#10919=CARTESIAN_POINT('Ctrl Pts',(2.25149501557585,16.9109641128297,3.13572794938478));
#10920=CARTESIAN_POINT('Ctrl Pts',(2.18478179494117,16.7826430194041,2.82892325157911));
#10921=CARTESIAN_POINT('Ctrl Pts',(2.1650635094611,16.75,2.66038133370061));
#10922=CARTESIAN_POINT('Ctrl Pts',(2.1650635094611,16.75,2.33961866629939));
#10923=CARTESIAN_POINT('Ctrl Pts',(2.18478179494117,16.7826430194041,2.17107674842089));
#10924=CARTESIAN_POINT('Ctrl Pts',(2.25149501557585,16.9109641128297,1.86427205061523));
#10925=CARTESIAN_POINT('Ctrl Pts',(2.29712558443605,17.0065552148362,1.72567783219742));
#10926=CARTESIAN_POINT('Ctrl Pts',(2.37983326258812,17.2253791627422,1.50685388429146));
#10927=CARTESIAN_POINT('Ctrl Pts',(2.42283105129935,17.364074052357,1.41104365009428));
#10928=CARTESIAN_POINT('Ctrl Pts',(2.48323996043832,17.6713186556389,1.28254511766359));
#10929=CARTESIAN_POINT('Ctrl Pts',(2.5,17.8400558736141,1.25));
#10930=CARTESIAN_POINT('Ctrl Pts',(2.5,18.,1.25));
#10931=CARTESIAN_POINT('',(-7.75,18.,3.75));
#10932=CARTESIAN_POINT('Origin',(0.,18.,2.));
#10933=CARTESIAN_POINT('Origin',(0.,18.,-2.));
#10934=CARTESIAN_POINT('',(-2.5,18.,-2.));
#10935=CARTESIAN_POINT('',(-2.5,18.,5.));
#10936=CARTESIAN_POINT('',(-2.5,18.,-2.));
#10937=CARTESIAN_POINT('Origin',(0.,18.,5.));
#10938=CARTESIAN_POINT('Origin',(0.,0.,5.));
#10939=CARTESIAN_POINT('Origin',(0.,0.,2.));
#10940=CARTESIAN_POINT('',(-1.5,-1.83697019872103E-16,2.));
#10941=CARTESIAN_POINT('Origin',(0.,0.,2.));
#10942=CARTESIAN_POINT('',(-1.5,-1.83697019872103E-16,-2.));
#10943=CARTESIAN_POINT('',(-1.5,-1.83697019872103E-16,2.));
#10944=CARTESIAN_POINT('Origin',(0.,0.,-2.));
#10945=CARTESIAN_POINT('Origin',(0.,0.,-2.));
#10946=CARTESIAN_POINT('',(1.25,0.,-2.));
#10947=CARTESIAN_POINT('Origin',(0.,0.,-2.));
#10948=CARTESIAN_POINT('',(0.,0.,0.));
#10949=CARTESIAN_POINT('Origin',(0.,-14.,0.));
#10950=CARTESIAN_POINT('',(1.83697019872103E-16,-14.,-1.5));
#10951=CARTESIAN_POINT('Origin',(0.,-14.,0.));
#10952=CARTESIAN_POINT('Origin',(0.,0.7,0.));
#10953=CARTESIAN_POINT('',(1.83697019872103E-16,-10.,-1.5));
#10954=CARTESIAN_POINT('',(1.83697019872103E-16,0.7,-1.5));
#10955=CARTESIAN_POINT('Origin',(0.,-10.,0.));
#10956=CARTESIAN_POINT('Origin',(0.,-10.,0.));
#10957=CARTESIAN_POINT('',(2.44929359829471E-16,-10.,-2.));
#10958=CARTESIAN_POINT('Origin',(0.,-10.,0.));
#10959=CARTESIAN_POINT('Origin',(0.,0.7,0.));
#10960=CARTESIAN_POINT('',(2.44929359829471E-16,-3.,-2.));
#10961=CARTESIAN_POINT('',(2.44929359829471E-16,0.7,-2.));
#10962=CARTESIAN_POINT('Origin',(0.,-3.,0.));
#10963=CARTESIAN_POINT('Origin',(0.,-3.,0.));
#10964=CARTESIAN_POINT('',(4.28626379701574E-16,-3.,-3.5));
#10965=CARTESIAN_POINT('Origin',(0.,-3.,0.));
#10966=CARTESIAN_POINT('Origin',(0.,0.7,0.));
#10967=CARTESIAN_POINT('',(4.28626379701574E-16,0.,-3.5));
#10968=CARTESIAN_POINT('',(4.28626379701574E-16,0.7,-3.5));
#10969=CARTESIAN_POINT('',(3.464101615138,0.,-0.5));
#10970=CARTESIAN_POINT('Origin',(0.,0.,0.));
#10971=CARTESIAN_POINT('',(3.464101615138,-1.,-0.5));
#10972=CARTESIAN_POINT('',(3.464101615138,0.,-0.5));
#10973=CARTESIAN_POINT('',(3.464101615138,-1.,0.5));
#10974=CARTESIAN_POINT('Origin',(0.,-1.,0.));
#10975=CARTESIAN_POINT('',(3.464101615138,0.,0.5));
#10976=CARTESIAN_POINT('',(3.464101615138,0.,0.5));
#10977=CARTESIAN_POINT('',(-3.464101615138,0.,0.5));
#10978=CARTESIAN_POINT('Origin',(0.,0.,0.));
#10979=CARTESIAN_POINT('',(-3.464101615138,-1.,0.5));
#10980=CARTESIAN_POINT('',(-3.464101615138,0.,0.5));
#10981=CARTESIAN_POINT('',(-3.464101615138,-1.,-0.5));
#10982=CARTESIAN_POINT('Origin',(0.,-1.,0.));
#10983=CARTESIAN_POINT('',(-3.464101615138,0.,-0.5));
#10984=CARTESIAN_POINT('',(-3.464101615138,0.,-0.5));
#10985=CARTESIAN_POINT('Origin',(0.,0.,0.));
#10986=CARTESIAN_POINT('Origin',(-5.15,0.,0.5));
#10987=CARTESIAN_POINT('',(-3.464101615138,-1.,0.5));
#10988=CARTESIAN_POINT('',(3.464101615138,0.,0.5));
#10989=CARTESIAN_POINT('Origin',(-5.15,-1.,0.5));
#10990=CARTESIAN_POINT('',(-3.464101615138,-1.,-0.5));
#10991=CARTESIAN_POINT('Origin',(-5.15,-1.,-0.5));
#10992=CARTESIAN_POINT('',(3.464101615138,0.,-0.5));
#10993=CARTESIAN_POINT('Origin',(0.,0.,0.));
#10994=CARTESIAN_POINT('Origin',(0.,0.,0.));
#10995=CARTESIAN_POINT('Origin',(0.,-14.,0.));
#10996=CARTESIAN_POINT('',(-1.25,-14.,-1.53080849893419E-16));
#10997=CARTESIAN_POINT('Origin',(0.,-14.,0.));
#10998=CARTESIAN_POINT('',(-1.25,-10.,-1.53080849893419E-16));
#10999=CARTESIAN_POINT('',(-1.25,-14.,-1.53080849893419E-16));
#11000=CARTESIAN_POINT('Origin',(0.,-10.,0.));
#11001=CARTESIAN_POINT('Origin',(0.,-10.,0.));
#11002=CARTESIAN_POINT('',(1.5,-10.,0.));
#11003=CARTESIAN_POINT('Origin',(0.,-10.,0.));
#11004=CARTESIAN_POINT('',(0.,0.,0.));
#11005=CARTESIAN_POINT('Origin',(0.,-22.5,0.));
#11006=CARTESIAN_POINT('',(-2.5,-22.5,0.));
#11007=CARTESIAN_POINT('Origin',(0.,-22.5,0.));
#11008=CARTESIAN_POINT('Origin',(0.,-22.5,0.));
#11009=CARTESIAN_POINT('',(-2.5,22.5,3.06161699786838E-16));
#11010=CARTESIAN_POINT('Origin',(0.,22.5,0.));
#11011=CARTESIAN_POINT('',(-2.5,19.75,6.63446760945788E-17));
#11012=CARTESIAN_POINT('',(-2.5,-22.5,3.06161699786838E-16));
#11013=CARTESIAN_POINT('',(-2.5,17.25,0.));
#11014=CARTESIAN_POINT('Ctrl Pts',(-2.5,17.25,3.12250225675825E-16));
#11015=CARTESIAN_POINT('Ctrl Pts',(-2.5,17.25,0.159944126385861));
#11016=CARTESIAN_POINT('Ctrl Pts',(-2.48323996043832,17.2825451176636,0.328681344361068));
#11017=CARTESIAN_POINT('Ctrl Pts',(-2.42283105129935,17.4110436500943,0.635925947642967));
#11018=CARTESIAN_POINT('Ctrl Pts',(-2.37983326258812,17.5068538842915,0.774620837257827));
#11019=CARTESIAN_POINT('Ctrl Pts',(-2.29712558443605,17.7256778321974,0.993444785163792));
#11020=CARTESIAN_POINT('Ctrl Pts',(-2.25149501557585,17.8642720506152,1.08903588717028));
#11021=CARTESIAN_POINT('Ctrl Pts',(-2.18478179494117,18.1710767484209,1.21735698059595));
#11022=CARTESIAN_POINT('Ctrl Pts',(-2.1650635094611,18.3396186662994,1.25));
#11023=CARTESIAN_POINT('Ctrl Pts',(-2.1650635094611,18.6603813337006,1.25));
#11024=CARTESIAN_POINT('Ctrl Pts',(-2.18478179494117,18.8289232515791,1.21735698059595));
#11025=CARTESIAN_POINT('Ctrl Pts',(-2.25149501557585,19.1357279493848,1.08903588717028));
#11026=CARTESIAN_POINT('Ctrl Pts',(-2.29712558443604,19.2743221678026,0.993444785163795));
#11027=CARTESIAN_POINT('Ctrl Pts',(-2.37983326258812,19.4931461157085,0.77462083725783));
#11028=CARTESIAN_POINT('Ctrl Pts',(-2.42283105129935,19.5889563499057,0.63592594764297));
#11029=CARTESIAN_POINT('Ctrl Pts',(-2.48323996043832,19.7174548823364,0.328681344361071));
#11030=CARTESIAN_POINT('Ctrl Pts',(-2.5,19.75,0.159944126385861));
#11031=CARTESIAN_POINT('Ctrl Pts',(-2.5,19.75,-3.46944695195361E-16));
#11032=CARTESIAN_POINT('',(-2.5,-17.75,1.35733615133651E-16));
#11033=CARTESIAN_POINT('',(-2.5,-22.5,3.06161699786838E-16));
#11034=CARTESIAN_POINT('',(-2.5,-20.25,0.));
#11035=CARTESIAN_POINT('Ctrl Pts',(-2.5,-20.25,1.73472347597681E-16));
#11036=CARTESIAN_POINT('Ctrl Pts',(-2.5,-20.25,0.159944126385861));
#11037=CARTESIAN_POINT('Ctrl Pts',(-2.48323996043832,-20.2174548823364,
0.32868134436107));
#11038=CARTESIAN_POINT('Ctrl Pts',(-2.42283105129935,-20.0889563499057,
0.635925947642969));
#11039=CARTESIAN_POINT('Ctrl Pts',(-2.37983326258812,-19.9931461157085,
0.774620837257828));
#11040=CARTESIAN_POINT('Ctrl Pts',(-2.29712558443605,-19.7743221678026,
0.993444785163793));
#11041=CARTESIAN_POINT('Ctrl Pts',(-2.25149501557585,-19.6357279493848,
1.08903588717028));
#11042=CARTESIAN_POINT('Ctrl Pts',(-2.18478179494117,-19.3289232515791,
1.21735698059595));
#11043=CARTESIAN_POINT('Ctrl Pts',(-2.1650635094611,-19.1603813337006,1.25));
#11044=CARTESIAN_POINT('Ctrl Pts',(-2.1650635094611,-18.8396186662994,1.25));
#11045=CARTESIAN_POINT('Ctrl Pts',(-2.18478179494117,-18.6710767484209,
1.21735698059595));
#11046=CARTESIAN_POINT('Ctrl Pts',(-2.25149501557585,-18.3642720506152,
1.08903588717028));
#11047=CARTESIAN_POINT('Ctrl Pts',(-2.29712558443605,-18.2256778321974,
0.993444785163793));
#11048=CARTESIAN_POINT('Ctrl Pts',(-2.37983326258812,-18.0068538842915,
0.774620837257828));
#11049=CARTESIAN_POINT('Ctrl Pts',(-2.42283105129935,-17.9110436500943,
0.635925947642967));
#11050=CARTESIAN_POINT('Ctrl Pts',(-2.48323996043832,-17.7825451176636,
0.328681344361068));
#11051=CARTESIAN_POINT('Ctrl Pts',(-2.5,-17.75,0.159944126385861));
#11052=CARTESIAN_POINT('Ctrl Pts',(-2.5,-17.75,2.77555756156289E-16));
#11053=CARTESIAN_POINT('',(-2.5,-22.5,3.06161699786838E-16));
#11054=CARTESIAN_POINT('Ctrl Pts',(-2.5,-17.75,-1.38777878078145E-16));
#11055=CARTESIAN_POINT('Ctrl Pts',(-2.5,-17.75,-0.159944126385861));
#11056=CARTESIAN_POINT('Ctrl Pts',(-2.48323996043832,-17.7825451176636,
-0.328681344361068));
#11057=CARTESIAN_POINT('Ctrl Pts',(-2.42283105129935,-17.9110436500943,
-0.635925947642967));
#11058=CARTESIAN_POINT('Ctrl Pts',(-2.37983326258812,-18.0068538842915,
-0.774620837257828));
#11059=CARTESIAN_POINT('Ctrl Pts',(-2.29712558443605,-18.2256778321974,
-0.993444785163793));
#11060=CARTESIAN_POINT('Ctrl Pts',(-2.25149501557585,-18.3642720506152,
-1.08903588717028));
#11061=CARTESIAN_POINT('Ctrl Pts',(-2.18478179494117,-18.6710767484209,
-1.21735698059595));
#11062=CARTESIAN_POINT('Ctrl Pts',(-2.1650635094611,-18.8396186662994,-1.25));
#11063=CARTESIAN_POINT('Ctrl Pts',(-2.1650635094611,-19.,-1.25));
#11064=CARTESIAN_POINT('Ctrl Pts',(-2.1650635094611,-19.1603813337006,-1.25));
#11065=CARTESIAN_POINT('Ctrl Pts',(-2.18478179494117,-19.3289232515791,
-1.21735698059595));
#11066=CARTESIAN_POINT('Ctrl Pts',(-2.25149501557585,-19.6357279493848,
-1.08903588717028));
#11067=CARTESIAN_POINT('Ctrl Pts',(-2.29712558443605,-19.7743221678026,
-0.993444785163793));
#11068=CARTESIAN_POINT('Ctrl Pts',(-2.37983326258812,-19.9931461157085,
-0.774620837257828));
#11069=CARTESIAN_POINT('Ctrl Pts',(-2.42283105129935,-20.0889563499057,
-0.635925947642969));
#11070=CARTESIAN_POINT('Ctrl Pts',(-2.48323996043832,-20.2174548823364,
-0.32868134436107));
#11071=CARTESIAN_POINT('Ctrl Pts',(-2.5,-20.25,-0.159944126385861));
#11072=CARTESIAN_POINT('Ctrl Pts',(-2.5,-20.25,-1.38777878078145E-16));
#11073=CARTESIAN_POINT('Ctrl Pts',(-2.5,19.75,-1.73472347597681E-16));
#11074=CARTESIAN_POINT('Ctrl Pts',(-2.5,19.75,-0.159944126385861));
#11075=CARTESIAN_POINT('Ctrl Pts',(-2.48323996043832,19.7174548823364,-0.328681344361069));
#11076=CARTESIAN_POINT('Ctrl Pts',(-2.42283105129935,19.5889563499057,-0.635925947642968));
#11077=CARTESIAN_POINT('Ctrl Pts',(-2.37983326258812,19.4931461157085,-0.77462083725783));
#11078=CARTESIAN_POINT('Ctrl Pts',(-2.29712558443604,19.2743221678026,-0.993444785163795));
#11079=CARTESIAN_POINT('Ctrl Pts',(-2.25149501557585,19.1357279493848,-1.08903588717028));
#11080=CARTESIAN_POINT('Ctrl Pts',(-2.18478179494117,18.8289232515791,-1.21735698059595));
#11081=CARTESIAN_POINT('Ctrl Pts',(-2.1650635094611,18.6603813337006,-1.25));
#11082=CARTESIAN_POINT('Ctrl Pts',(-2.1650635094611,18.5,-1.25));
#11083=CARTESIAN_POINT('Ctrl Pts',(-2.1650635094611,18.3396186662994,-1.25));
#11084=CARTESIAN_POINT('Ctrl Pts',(-2.18478179494117,18.1710767484209,-1.21735698059595));
#11085=CARTESIAN_POINT('Ctrl Pts',(-2.25149501557585,17.8642720506152,-1.08903588717028));
#11086=CARTESIAN_POINT('Ctrl Pts',(-2.29712558443605,17.7256778321974,-0.993444785163791));
#11087=CARTESIAN_POINT('Ctrl Pts',(-2.37983326258812,17.5068538842915,-0.774620837257827));
#11088=CARTESIAN_POINT('Ctrl Pts',(-2.42283105129935,17.4110436500943,-0.635925947642967));
#11089=CARTESIAN_POINT('Ctrl Pts',(-2.48323996043832,17.2825451176636,-0.328681344361068));
#11090=CARTESIAN_POINT('Ctrl Pts',(-2.5,17.25,-0.15994412638586));
#11091=CARTESIAN_POINT('Ctrl Pts',(-2.5,17.25,2.42861286636753E-16));
#11092=CARTESIAN_POINT('',(2.5,17.25,0.));
#11093=CARTESIAN_POINT('',(2.5,19.75,4.92874059181143E-16));
#11094=CARTESIAN_POINT('Ctrl Pts',(2.5,17.25,-1.38777878078145E-16));
#11095=CARTESIAN_POINT('Ctrl Pts',(2.5,17.25,-0.159944126385861));
#11096=CARTESIAN_POINT('Ctrl Pts',(2.48323996043832,17.2825451176636,-0.328681344361068));
#11097=CARTESIAN_POINT('Ctrl Pts',(2.42283105129935,17.4110436500943,-0.635925947642967));
#11098=CARTESIAN_POINT('Ctrl Pts',(2.37983326258812,17.5068538842915,-0.774620837257827));
#11099=CARTESIAN_POINT('Ctrl Pts',(2.29712558443605,17.7256778321974,-0.993444785163792));
#11100=CARTESIAN_POINT('Ctrl Pts',(2.25149501557585,17.8642720506152,-1.08903588717028));
#11101=CARTESIAN_POINT('Ctrl Pts',(2.18478179494117,18.1710767484209,-1.21735698059595));
#11102=CARTESIAN_POINT('Ctrl Pts',(2.1650635094611,18.3396186662994,-1.25));
#11103=CARTESIAN_POINT('Ctrl Pts',(2.1650635094611,18.5,-1.25));
#11104=CARTESIAN_POINT('Ctrl Pts',(2.1650635094611,18.6603813337006,-1.25));
#11105=CARTESIAN_POINT('Ctrl Pts',(2.18478179494117,18.8289232515791,-1.21735698059595));
#11106=CARTESIAN_POINT('Ctrl Pts',(2.25149501557585,19.1357279493848,-1.08903588717028));
#11107=CARTESIAN_POINT('Ctrl Pts',(2.29712558443604,19.2743221678026,-0.993444785163795));
#11108=CARTESIAN_POINT('Ctrl Pts',(2.37983326258812,19.4931461157085,-0.77462083725783));
#11109=CARTESIAN_POINT('Ctrl Pts',(2.42283105129935,19.5889563499057,-0.635925947642969));
#11110=CARTESIAN_POINT('Ctrl Pts',(2.48323996043832,19.7174548823364,-0.32868134436107));
#11111=CARTESIAN_POINT('Ctrl Pts',(2.5,19.75,-0.159944126385861));
#11112=CARTESIAN_POINT('Ctrl Pts',(2.5,19.75,1.04083408558608E-16));
#11113=CARTESIAN_POINT('Ctrl Pts',(2.5,19.75,1.73472347597681E-16));
#11114=CARTESIAN_POINT('Ctrl Pts',(2.5,19.75,0.159944126385861));
#11115=CARTESIAN_POINT('Ctrl Pts',(2.48323996043832,19.7174548823364,0.328681344361071));
#11116=CARTESIAN_POINT('Ctrl Pts',(2.42283105129935,19.5889563499057,0.63592594764297));
#11117=CARTESIAN_POINT('Ctrl Pts',(2.37983326258812,19.4931461157085,0.77462083725783));
#11118=CARTESIAN_POINT('Ctrl Pts',(2.29712558443604,19.2743221678026,0.993444785163795));
#11119=CARTESIAN_POINT('Ctrl Pts',(2.25149501557585,19.1357279493848,1.08903588717028));
#11120=CARTESIAN_POINT('Ctrl Pts',(2.18478179494117,18.8289232515791,1.21735698059595));
#11121=CARTESIAN_POINT('Ctrl Pts',(2.1650635094611,18.6603813337006,1.25));
#11122=CARTESIAN_POINT('Ctrl Pts',(2.1650635094611,18.3396186662994,1.25));
#11123=CARTESIAN_POINT('Ctrl Pts',(2.18478179494117,18.1710767484209,1.21735698059595));
#11124=CARTESIAN_POINT('Ctrl Pts',(2.25149501557585,17.8642720506152,1.08903588717028));
#11125=CARTESIAN_POINT('Ctrl Pts',(2.29712558443605,17.7256778321974,0.993444785163791));
#11126=CARTESIAN_POINT('Ctrl Pts',(2.37983326258812,17.5068538842915,0.774620837257827));
#11127=CARTESIAN_POINT('Ctrl Pts',(2.42283105129935,17.4110436500943,0.635925947642967));
#11128=CARTESIAN_POINT('Ctrl Pts',(2.48323996043832,17.2825451176636,0.328681344361068));
#11129=CARTESIAN_POINT('Ctrl Pts',(2.5,17.25,0.159944126385861));
#11130=CARTESIAN_POINT('Ctrl Pts',(2.5,17.25,1.04083408558608E-16));
#11131=CARTESIAN_POINT('',(2.5,-17.75,0.));
#11132=CARTESIAN_POINT('Ctrl Pts',(2.1650635094611,-19.,-1.25));
#11133=CARTESIAN_POINT('Ctrl Pts',(2.1650635094611,-18.8396186662994,-1.25));
#11134=CARTESIAN_POINT('Ctrl Pts',(2.18478179494117,-18.6710767484209,-1.21735698059595));
#11135=CARTESIAN_POINT('Ctrl Pts',(2.25149501557585,-18.3642720506152,-1.08903588717028));
#11136=CARTESIAN_POINT('Ctrl Pts',(2.29712558443605,-18.2256778321974,-0.993444785163793));
#11137=CARTESIAN_POINT('Ctrl Pts',(2.37983326258812,-18.0068538842915,-0.774620837257828));
#11138=CARTESIAN_POINT('Ctrl Pts',(2.42283105129935,-17.9110436500943,-0.63592594764297));
#11139=CARTESIAN_POINT('Ctrl Pts',(2.48323996043832,-17.7825451176636,-0.328681344361071));
#11140=CARTESIAN_POINT('Ctrl Pts',(2.5,-17.75,-0.159944126385861));
#11141=CARTESIAN_POINT('Ctrl Pts',(2.5,-17.75,0.159944126385861));
#11142=CARTESIAN_POINT('Ctrl Pts',(2.48323996043832,-17.7825451176636,0.328681344361068));
#11143=CARTESIAN_POINT('Ctrl Pts',(2.42283105129935,-17.9110436500943,0.635925947642967));
#11144=CARTESIAN_POINT('Ctrl Pts',(2.37983326258812,-18.0068538842915,0.774620837257829));
#11145=CARTESIAN_POINT('Ctrl Pts',(2.29712558443605,-18.2256778321974,0.993444785163793));
#11146=CARTESIAN_POINT('Ctrl Pts',(2.25149501557585,-18.3642720506152,1.08903588717028));
#11147=CARTESIAN_POINT('Ctrl Pts',(2.18478179494117,-18.6710767484209,1.21735698059595));
#11148=CARTESIAN_POINT('Ctrl Pts',(2.1650635094611,-18.8396186662994,1.25));
#11149=CARTESIAN_POINT('Ctrl Pts',(2.1650635094611,-19.1603813337006,1.25));
#11150=CARTESIAN_POINT('Ctrl Pts',(2.18478179494117,-19.3289232515791,1.21735698059595));
#11151=CARTESIAN_POINT('Ctrl Pts',(2.25149501557585,-19.6357279493848,1.08903588717028));
#11152=CARTESIAN_POINT('Ctrl Pts',(2.29712558443605,-19.7743221678026,0.993444785163793));
#11153=CARTESIAN_POINT('Ctrl Pts',(2.37983326258812,-19.9931461157085,0.774620837257828));
#11154=CARTESIAN_POINT('Ctrl Pts',(2.42283105129935,-20.0889563499057,0.635925947642968));
#11155=CARTESIAN_POINT('Ctrl Pts',(2.48323996043832,-20.2174548823364,0.328681344361069));
#11156=CARTESIAN_POINT('Ctrl Pts',(2.5,-20.25,0.159944126385861));
#11157=CARTESIAN_POINT('Ctrl Pts',(2.5,-20.25,-0.159944126385861));
#11158=CARTESIAN_POINT('Ctrl Pts',(2.48323996043832,-20.2174548823364,-0.32868134436107));
#11159=CARTESIAN_POINT('Ctrl Pts',(2.42283105129935,-20.0889563499057,-0.635925947642969));
#11160=CARTESIAN_POINT('Ctrl Pts',(2.37983326258812,-19.9931461157085,-0.774620837257828));
#11161=CARTESIAN_POINT('Ctrl Pts',(2.29712558443605,-19.7743221678026,-0.993444785163793));
#11162=CARTESIAN_POINT('Ctrl Pts',(2.25149501557585,-19.6357279493848,-1.08903588717028));
#11163=CARTESIAN_POINT('Ctrl Pts',(2.18478179494117,-19.3289232515791,-1.21735698059595));
#11164=CARTESIAN_POINT('Ctrl Pts',(2.1650635094611,-19.1603813337006,-1.25));
#11165=CARTESIAN_POINT('Ctrl Pts',(2.1650635094611,-19.,-1.25));
#11166=CARTESIAN_POINT('Origin',(-6.,18.5,0.));
#11167=CARTESIAN_POINT('',(6.,19.75,1.53080849893419E-16));
#11168=CARTESIAN_POINT('Origin',(6.,18.5,0.));
#11169=CARTESIAN_POINT('',(-6.,19.75,1.53080849893419E-16));
#11170=CARTESIAN_POINT('Origin',(-6.,18.5,0.));
#11171=CARTESIAN_POINT('',(-6.,19.75,0.));
#11172=CARTESIAN_POINT('',(-6.,19.75,1.53080849893419E-16));
#11173=CARTESIAN_POINT('Origin',(-6.,18.5,0.));
#11174=CARTESIAN_POINT('Origin',(0.,22.5,0.));
#11175=CARTESIAN_POINT('Origin',(-6.,-19.,0.));
#11176=CARTESIAN_POINT('',(-6.,-17.75,1.53080849893419E-16));
#11177=CARTESIAN_POINT('',(-6.,-17.75,1.53080849893419E-16));
#11178=CARTESIAN_POINT('Origin',(-6.,-19.,0.));
#11179=CARTESIAN_POINT('Origin',(-6.,-19.,0.));
#11180=CARTESIAN_POINT('',(6.,-17.75,0.));
#11181=CARTESIAN_POINT('Origin',(6.,-19.,0.));
#11182=CARTESIAN_POINT('',(-6.,-17.75,1.53080849893419E-16));
#11183=CARTESIAN_POINT('Origin',(6.,0.,0.));
#11184=CARTESIAN_POINT('Origin',(6.,0.,0.));
#11185=CARTESIAN_POINT('Origin',(-6.,0.,0.));
#11186=CARTESIAN_POINT('Origin',(-6.,0.,0.));
#11187=CARTESIAN_POINT('',(0.,0.,0.));
#11188=CARTESIAN_POINT('',(0.,0.,-12.));
#11189=CARTESIAN_POINT('',(0.,18.,21.));
#11190=CARTESIAN_POINT('',(0.,0.,0.));
#11191=CARTESIAN_POINT('',(0.,34.,18.));
#11192=CARTESIAN_POINT('',(0.,0.,0.));
#11193=CARTESIAN_POINT('',(0.,0.,0.));
#11194=CARTESIAN_POINT('Origin',(0.,0.,0.));
#11195=CARTESIAN_POINT('',(0.,-10.,0.));
#11196=CARTESIAN_POINT('',(14.,-10.,0.));
#11197=CARTESIAN_POINT('',(0.,-10.,0.));
#11198=CARTESIAN_POINT('',(14.,10.,0.));
#11199=CARTESIAN_POINT('',(14.,10.,0.));
#11200=CARTESIAN_POINT('',(0.,10.,0.));
#11201=CARTESIAN_POINT('',(14.,10.,0.));
#11202=CARTESIAN_POINT('Origin',(0.,0.,0.));
#11203=CARTESIAN_POINT('Origin',(-0.133704,-10.,-0.5));
#11204=CARTESIAN_POINT('',(14.,-10.5,-0.5));
#11205=CARTESIAN_POINT('Origin',(14.,-10.,-0.5));
#11206=CARTESIAN_POINT('',(2.205697222091E-10,-10.5,-0.5));
#11207=CARTESIAN_POINT('Origin',(0.,-10.,-0.5));
#11208=CARTESIAN_POINT('',(2.205697222091E-10,-10.5,-0.5));
#11209=CARTESIAN_POINT('Origin',(14.,0.,0.));
#11210=CARTESIAN_POINT('',(14.,-10.5,-28.));
#11211=CARTESIAN_POINT('',(14.,-10.5,-0.5));
#11212=CARTESIAN_POINT('',(14.,10.5,-28.));
#11213=CARTESIAN_POINT('',(14.,-10.5,-28.));
#11214=CARTESIAN_POINT('',(14.,10.5,-0.5));
#11215=CARTESIAN_POINT('',(14.,10.5,-28.));
#11216=CARTESIAN_POINT('Origin',(14.,10.,-0.5));
#11217=CARTESIAN_POINT('',(14.,0.,-24.));
#11218=CARTESIAN_POINT('Origin',(14.,0.,-22.));
#11219=CARTESIAN_POINT('',(14.,1.75,-7.));
#11220=CARTESIAN_POINT('Origin',(14.,0.,-7.));
#11221=CARTESIAN_POINT('Origin',(0.,0.,-7.));
#11222=CARTESIAN_POINT('',(7.806247497998,-1.75,-7.));
#11223=CARTESIAN_POINT('',(7.806247497998,1.75,-7.));
#11224=CARTESIAN_POINT('Ctrl Pts',(7.806247497998,-1.75,-7.));
#11225=CARTESIAN_POINT('Ctrl Pts',(7.806247497998,-1.75,-7.22051202732056));
#11226=CARTESIAN_POINT('Ctrl Pts',(7.81656151369615,-1.70578419252538,-7.45521537354111));
#11227=CARTESIAN_POINT('Ctrl Pts',(7.85345055027074,-1.52697344069322,-7.8861563440924));
#11228=CARTESIAN_POINT('Ctrl Pts',(7.8794534058773,-1.3924155896664,-8.08245814448651));
#11229=CARTESIAN_POINT('Ctrl Pts',(7.9279795931108,-1.08247066684372,-8.39240306730919));
#11230=CARTESIAN_POINT('Ctrl Pts',(7.95370820844925,-0.886163584469686,
-8.52697071250845));
#11231=CARTESIAN_POINT('Ctrl Pts',(7.98996554209154,-0.455204126605999,
-8.7057885831527));
#11232=CARTESIAN_POINT('Ctrl Pts',(8.,-0.220494209840019,-8.75));
#11233=CARTESIAN_POINT('Ctrl Pts',(8.,0.220494209840019,-8.75));
#11234=CARTESIAN_POINT('Ctrl Pts',(7.98996554209154,0.455204126605999,-8.7057885831527));
#11235=CARTESIAN_POINT('Ctrl Pts',(7.95370820844925,0.886163584469686,-8.52697071250845));
#11236=CARTESIAN_POINT('Ctrl Pts',(7.9279795931108,1.08247066684372,-8.39240306730919));
#11237=CARTESIAN_POINT('Ctrl Pts',(7.8794534058773,1.3924155896664,-8.08245814448651));
#11238=CARTESIAN_POINT('Ctrl Pts',(7.85345055027074,1.52697344069322,-7.8861563440924));
#11239=CARTESIAN_POINT('Ctrl Pts',(7.81656151369615,1.70578419252538,-7.45521537354111));
#11240=CARTESIAN_POINT('Ctrl Pts',(7.806247497998,1.75,-7.22051202732056));
#11241=CARTESIAN_POINT('Ctrl Pts',(7.806247497998,1.75,-7.));
#11242=CARTESIAN_POINT('Ctrl Pts',(7.806247497998,1.75,-7.));
#11243=CARTESIAN_POINT('Ctrl Pts',(7.806247497998,1.75,-6.77948797267944));
#11244=CARTESIAN_POINT('Ctrl Pts',(7.81656151369615,1.70578419252538,-6.5447846264589));
#11245=CARTESIAN_POINT('Ctrl Pts',(7.85345055027074,1.52697344069322,-6.1138436559076));
#11246=CARTESIAN_POINT('Ctrl Pts',(7.8794534058773,1.3924155896664,-5.91754185551349));
#11247=CARTESIAN_POINT('Ctrl Pts',(7.9279795931108,1.08247066684372,-5.60759693269081));
#11248=CARTESIAN_POINT('Ctrl Pts',(7.95370820844925,0.886163584469687,-5.47302928749155));
#11249=CARTESIAN_POINT('Ctrl Pts',(7.98996554209154,0.455204126606001,-5.2942114168473));
#11250=CARTESIAN_POINT('Ctrl Pts',(8.,0.220494209840019,-5.25));
#11251=CARTESIAN_POINT('Ctrl Pts',(8.,-0.220494209840019,-5.25));
#11252=CARTESIAN_POINT('Ctrl Pts',(7.98996554209154,-0.455204126606001,
-5.2942114168473));
#11253=CARTESIAN_POINT('Ctrl Pts',(7.95370820844925,-0.886163584469688,
-5.47302928749155));
#11254=CARTESIAN_POINT('Ctrl Pts',(7.9279795931108,-1.08247066684372,-5.60759693269081));
#11255=CARTESIAN_POINT('Ctrl Pts',(7.8794534058773,-1.3924155896664,-5.91754185551349));
#11256=CARTESIAN_POINT('Ctrl Pts',(7.85345055027074,-1.52697344069322,-6.1138436559076));
#11257=CARTESIAN_POINT('Ctrl Pts',(7.81656151369615,-1.70578419252538,-6.5447846264589));
#11258=CARTESIAN_POINT('Ctrl Pts',(7.806247497998,-1.75,-6.77948797267944));
#11259=CARTESIAN_POINT('Ctrl Pts',(7.806247497998,-1.75,-7.));
#11260=CARTESIAN_POINT('',(0.,1.75,-7.));
#11261=CARTESIAN_POINT('Origin',(0.,0.,-55.));
#11262=CARTESIAN_POINT('',(0.,8.,-3.));
#11263=CARTESIAN_POINT('Origin',(0.,0.,-3.));
#11264=CARTESIAN_POINT('',(0.,8.,-55.));
#11265=CARTESIAN_POINT('',(9.79717439317883E-16,8.,-55.));
#11266=CARTESIAN_POINT('Origin',(0.,0.,-55.));
#11267=CARTESIAN_POINT('',(7.745966692415,-2.,-48.));
#11268=CARTESIAN_POINT('',(7.74596669241483,2.,-48.));
#11269=CARTESIAN_POINT('Ctrl Pts',(7.74596669241483,-2.,-48.));
#11270=CARTESIAN_POINT('Ctrl Pts',(7.74596669241483,-2.,-48.2522988213568));
#11271=CARTESIAN_POINT('Ctrl Pts',(7.75957726931369,-1.94935810817991,-48.520643416021));
#11272=CARTESIAN_POINT('Ctrl Pts',(7.8080895555786,-1.74492797023227,-49.0130613700609));
#11273=CARTESIAN_POINT('Ctrl Pts',(7.84222121032682,-1.59119421565163,-49.2372329090946));
#11274=CARTESIAN_POINT('Ctrl Pts',(7.90579009335489,-1.23725765414306,-49.5911694706031));
#11275=CARTESIAN_POINT('Ctrl Pts',(7.93945007560674,-1.01307580920409,-49.7449225186146));
#11276=CARTESIAN_POINT('Ctrl Pts',(7.98687320195912,-0.52062131163299,-49.9493667420601));
#11277=CARTESIAN_POINT('Ctrl Pts',(8.,-0.252263545486473,-50.));
#11278=CARTESIAN_POINT('Ctrl Pts',(8.,0.252263545486474,-50.));
#11279=CARTESIAN_POINT('Ctrl Pts',(7.98687320195912,0.520621311632991,-49.9493667420601));
#11280=CARTESIAN_POINT('Ctrl Pts',(7.93945007560674,1.01307580920409,-49.7449225186146));
#11281=CARTESIAN_POINT('Ctrl Pts',(7.90579009335489,1.23725765414306,-49.5911694706031));
#11282=CARTESIAN_POINT('Ctrl Pts',(7.84222121032682,1.59119421565164,-49.2372329090946));
#11283=CARTESIAN_POINT('Ctrl Pts',(7.8080895555786,1.74492797023227,-49.0130613700609));
#11284=CARTESIAN_POINT('Ctrl Pts',(7.75957726931369,1.94935810817991,-48.520643416021));
#11285=CARTESIAN_POINT('Ctrl Pts',(7.74596669241483,2.,-48.2522988213568));
#11286=CARTESIAN_POINT('Ctrl Pts',(7.74596669241483,2.,-48.));
#11287=CARTESIAN_POINT('Ctrl Pts',(7.74596669241483,2.,-48.));
#11288=CARTESIAN_POINT('Ctrl Pts',(7.74596669241483,2.,-47.7477011786432));
#11289=CARTESIAN_POINT('Ctrl Pts',(7.75957726931369,1.94935810817991,-47.479356583979));
#11290=CARTESIAN_POINT('Ctrl Pts',(7.8080895555786,1.74492797023228,-46.9869386299392));
#11291=CARTESIAN_POINT('Ctrl Pts',(7.84222121032682,1.59119421565164,-46.7627670909054));
#11292=CARTESIAN_POINT('Ctrl Pts',(7.90579009335489,1.23725765414306,-46.4088305293969));
#11293=CARTESIAN_POINT('Ctrl Pts',(7.93945007560674,1.01307580920409,-46.2550774813855));
#11294=CARTESIAN_POINT('Ctrl Pts',(7.98687320195912,0.520621311632997,-46.0506332579399));
#11295=CARTESIAN_POINT('Ctrl Pts',(8.,0.252263545486474,-46.));
#11296=CARTESIAN_POINT('Ctrl Pts',(8.,-0.252263545486474,-46.));
#11297=CARTESIAN_POINT('Ctrl Pts',(7.98687320195912,-0.520621311632997,
-46.0506332579399));
#11298=CARTESIAN_POINT('Ctrl Pts',(7.93945007560674,-1.01307580920409,-46.2550774813855));
#11299=CARTESIAN_POINT('Ctrl Pts',(7.90579009335489,-1.23725765414306,-46.4088305293969));
#11300=CARTESIAN_POINT('Ctrl Pts',(7.84222121032682,-1.59119421565164,-46.7627670909054));
#11301=CARTESIAN_POINT('Ctrl Pts',(7.8080895555786,-1.74492797023227,-46.9869386299391));
#11302=CARTESIAN_POINT('Ctrl Pts',(7.75957726931369,-1.94935810817991,-47.479356583979));
#11303=CARTESIAN_POINT('Ctrl Pts',(7.74596669241483,-2.,-47.7477011786432));
#11304=CARTESIAN_POINT('Ctrl Pts',(7.74596669241483,-2.,-48.));
#11305=CARTESIAN_POINT('Origin',(0.,0.,-55.));
#11306=CARTESIAN_POINT('',(0.,16.,-55.));
#11307=CARTESIAN_POINT('Origin',(0.,0.,-55.));
#11308=CARTESIAN_POINT('',(-14.25,0.,-55.));
#11309=CARTESIAN_POINT('Origin',(-13.,0.,-55.));
#11310=CARTESIAN_POINT('',(5.678203230276,-11.,-55.));
#11311=CARTESIAN_POINT('Origin',(6.928203230276,-11.,-55.));
#11312=CARTESIAN_POINT('',(5.678203230276,11.,-55.));
#11313=CARTESIAN_POINT('Origin',(6.928203230276,11.,-55.));
#11314=CARTESIAN_POINT('Origin',(0.,0.,2.75));
#11315=CARTESIAN_POINT('',(0.,16.,-51.5));
#11316=CARTESIAN_POINT('',(1.95943487863577E-15,16.,2.75));
#11317=CARTESIAN_POINT('',(0.161181273708004,-15.9991881230582,-51.5));
#11318=CARTESIAN_POINT('Origin',(0.,0.,-51.5));
#11319=CARTESIAN_POINT('Origin',(0.,0.,-51.5));
#11320=CARTESIAN_POINT('Origin',(0.,0.,-51.5));
#11321=CARTESIAN_POINT('',(0.156144358904629,-15.4992134942126,-51.));
#11322=CARTESIAN_POINT('Origin',(0.156144358904629,-15.4992134942126,-51.5));
#11323=CARTESIAN_POINT('Origin',(0.,0.,-51.));
#11324=CARTESIAN_POINT('Origin',(0.,0.,-51.));
#11325=CARTESIAN_POINT('',(5.678203230276,-11.,-51.));
#11326=CARTESIAN_POINT('Origin',(6.928203230276,-11.,-51.));
#11327=CARTESIAN_POINT('',(5.678203230276,11.,-51.));
#11328=CARTESIAN_POINT('Origin',(6.928203230276,11.,-51.));
#11329=CARTESIAN_POINT('',(-0.228821208477847,-10.9976197813232,-51.));
#11330=CARTESIAN_POINT('Origin',(0.,0.,-51.));
#11331=CARTESIAN_POINT('',(-14.25,0.,-51.));
#11332=CARTESIAN_POINT('Origin',(-13.,0.,-51.));
#11333=CARTESIAN_POINT('Origin',(-13.,0.,-55.));
#11334=CARTESIAN_POINT('',(-14.25,1.53080849893419E-16,-55.));
#11335=CARTESIAN_POINT('Origin',(6.928203230276,-11.,-55.));
#11336=CARTESIAN_POINT('',(5.678203230276,-11.,-55.));
#11337=CARTESIAN_POINT('Origin',(6.928203230276,11.,-55.));
#11338=CARTESIAN_POINT('',(5.678203230276,11.,-55.));
#11339=CARTESIAN_POINT('Origin',(0.,0.,-50.5));
#11340=CARTESIAN_POINT('',(-0.218420244456127,-10.4977279730812,-50.5));
#11341=CARTESIAN_POINT('Origin',(-0.228821208477847,-10.9976197813232,-50.5));
#11342=CARTESIAN_POINT('',(0.,10.5,-50.5));
#11343=CARTESIAN_POINT('Origin',(0.,0.,-50.5));
#11344=CARTESIAN_POINT('Origin',(0.,0.,-50.5));
#11345=CARTESIAN_POINT('Origin',(0.,0.,2.75));
#11346=CARTESIAN_POINT('',(0.,10.4999999995,-28.5));
#11347=CARTESIAN_POINT('',(1.28587913910472E-15,10.5,2.75));
#11348=CARTESIAN_POINT('',(2.58748336760221E-14,-10.4999999995,-28.5));
#11349=CARTESIAN_POINT('Origin',(0.,0.,-28.5));
#11350=CARTESIAN_POINT('',(2.587483367663E-14,-10.49999999962,-28.5));
#11351=CARTESIAN_POINT('',(0.,10.5,-0.5));
#11352=CARTESIAN_POINT('Origin',(0.,0.,-0.5));
#11353=CARTESIAN_POINT('',(8.034813416777E-10,10.5,-0.5));
#11354=CARTESIAN_POINT('',(10.30776406404,2.,-48.));
#11355=CARTESIAN_POINT('Ctrl Pts',(10.3077640640442,-2.,-48.));
#11356=CARTESIAN_POINT('Ctrl Pts',(10.3077640640442,-2.,-47.7482070465008));
#11357=CARTESIAN_POINT('Ctrl Pts',(10.3179460772103,-1.94955285220986,-47.4800636214909));
#11358=CARTESIAN_POINT('Ctrl Pts',(10.3544601248255,-1.74525726713758,-46.9874944768476));
#11359=CARTESIAN_POINT('Ctrl Pts',(10.380236242486,-1.59144134502885,-46.7630142202827));
#11360=CARTESIAN_POINT('Ctrl Pts',(10.4284146976182,-1.2369939207975,-46.4085667960513));
#11361=CARTESIAN_POINT('Ctrl Pts',(10.4539852161582,-1.01251019566121,-46.2547444939347));
#11362=CARTESIAN_POINT('Ctrl Pts',(10.4900265771226,-0.519929037363746,
-46.050444279888));
#11363=CARTESIAN_POINT('Ctrl Pts',(10.5,-0.251781387216632,-46.));
#11364=CARTESIAN_POINT('Ctrl Pts',(10.5,0.251781387216631,-46.));
#11365=CARTESIAN_POINT('Ctrl Pts',(10.4900265771226,0.519929037363749,-46.050444279888));
#11366=CARTESIAN_POINT('Ctrl Pts',(10.4539852161582,1.01251019566121,-46.2547444939347));
#11367=CARTESIAN_POINT('Ctrl Pts',(10.4284146976182,1.2369939207975,-46.4085667960513));
#11368=CARTESIAN_POINT('Ctrl Pts',(10.380236242486,1.59144134502885,-46.7630142202827));
#11369=CARTESIAN_POINT('Ctrl Pts',(10.3544601248255,1.74525726713758,-46.9874944768476));
#11370=CARTESIAN_POINT('Ctrl Pts',(10.3179460772103,1.94955285220986,-47.4800636214909));
#11371=CARTESIAN_POINT('Ctrl Pts',(10.3077640640442,2.,-47.7482070465008));
#11372=CARTESIAN_POINT('Ctrl Pts',(10.3077640640442,2.,-48.2517929534992));
#11373=CARTESIAN_POINT('Ctrl Pts',(10.3179460772103,1.94955285220986,-48.5199363785091));
#11374=CARTESIAN_POINT('Ctrl Pts',(10.3544601248255,1.74525726713758,-49.0125055231524));
#11375=CARTESIAN_POINT('Ctrl Pts',(10.380236242486,1.59144134502885,-49.2369857797173));
#11376=CARTESIAN_POINT('Ctrl Pts',(10.4284146976182,1.2369939207975,-49.5914332039487));
#11377=CARTESIAN_POINT('Ctrl Pts',(10.4539852161582,1.01251019566121,-49.7452555060653));
#11378=CARTESIAN_POINT('Ctrl Pts',(10.4900265771226,0.519929037363747,-49.949555720112));
#11379=CARTESIAN_POINT('Ctrl Pts',(10.5,0.251781387216632,-50.));
#11380=CARTESIAN_POINT('Ctrl Pts',(10.5,-0.251781387216631,-50.));
#11381=CARTESIAN_POINT('Ctrl Pts',(10.4900265771226,-0.519929037363746,
-49.949555720112));
#11382=CARTESIAN_POINT('Ctrl Pts',(10.4539852161582,-1.01251019566121,-49.7452555060653));
#11383=CARTESIAN_POINT('Ctrl Pts',(10.4284146976182,-1.23699392079749,-49.5914332039487));
#11384=CARTESIAN_POINT('Ctrl Pts',(10.380236242486,-1.59144134502885,-49.2369857797173));
#11385=CARTESIAN_POINT('Ctrl Pts',(10.3544601248255,-1.74525726713758,-49.0125055231524));
#11386=CARTESIAN_POINT('Ctrl Pts',(10.3179460772103,-1.94955285220986,-48.5199363785091));
#11387=CARTESIAN_POINT('Ctrl Pts',(10.3077640640442,-2.,-48.2517929534992));
#11388=CARTESIAN_POINT('Ctrl Pts',(10.3077640640442,-2.,-48.));
#11389=CARTESIAN_POINT('Origin',(0.,0.,-48.));
#11390=CARTESIAN_POINT('',(0.,2.,-48.));
#11391=CARTESIAN_POINT('Origin',(0.,0.,-28.5));
#11392=CARTESIAN_POINT('',(3.27871926200197,-10.4999999995227,-28.));
#11393=CARTESIAN_POINT('',(3.27871926199412,10.4999999995103,-28.));
#11394=CARTESIAN_POINT('Origin',(0.,0.,-28.));
#11395=CARTESIAN_POINT('Ctrl Pts',(2.46987048725666E-14,-10.5,-28.5));
#11396=CARTESIAN_POINT('Ctrl Pts',(1.01790369883751,-10.5,-28.2778752023763));
#11397=CARTESIAN_POINT('Ctrl Pts',(2.23686160569662,-10.5,-28.));
#11398=CARTESIAN_POINT('Ctrl Pts',(3.27871925711855,-10.5,-28.));
#11399=CARTESIAN_POINT('Ctrl Pts',(3.27871925711855,10.5,-28.));
#11400=CARTESIAN_POINT('Ctrl Pts',(2.23686160569662,10.5,-27.9999999990974));
#11401=CARTESIAN_POINT('Ctrl Pts',(1.01790369883749,10.5,-28.2778752023763));
#11402=CARTESIAN_POINT('Ctrl Pts',(0.,10.5,-28.5));
#11403=CARTESIAN_POINT('Origin',(14.,-10.5,-28.));
#11404=CARTESIAN_POINT('',(14.,10.5,-28.));
#11405=CARTESIAN_POINT('',(14.,-10.5,-28.));
#11406=CARTESIAN_POINT('Origin',(14.,-10.5,0.));
#11407=CARTESIAN_POINT('Origin',(0.,0.,-0.5));
#11408=CARTESIAN_POINT('Origin',(0.,10.,-0.5));
#11409=CARTESIAN_POINT('Origin',(122.216,10.,-0.5));
#11410=CARTESIAN_POINT('',(14.,10.5,-0.5));
#11411=CARTESIAN_POINT('Origin',(14.,10.5,-28.));
#11412=CARTESIAN_POINT('Origin',(0.,0.,-3.));
#11413=CARTESIAN_POINT('Origin',(7.,0.,-22.));
#11414=CARTESIAN_POINT('',(49.,0.,-24.));
#11415=CARTESIAN_POINT('Origin',(49.,0.,-22.));
#11416=CARTESIAN_POINT('',(7.,2.44929359829471E-16,-24.));
#11417=CARTESIAN_POINT('Origin',(49.,0.,-22.));
#11418=CARTESIAN_POINT('Origin',(6.928203230276,-11.,-55.));
#11419=CARTESIAN_POINT('',(8.428203230276,-11.,-55.));
#11420=CARTESIAN_POINT('Origin',(6.928203230276,-11.,-55.));
#11421=CARTESIAN_POINT('',(8.428203230276,-11.,-51.));
#11422=CARTESIAN_POINT('',(8.428203230276,-11.,-55.));
#11423=CARTESIAN_POINT('Origin',(6.928203230276,-11.,-51.));
#11424=CARTESIAN_POINT('Origin',(6.928203230276,-11.,-51.));
#11425=CARTESIAN_POINT('',(5.678203230276,-11.,-51.));
#11426=CARTESIAN_POINT('Origin',(6.928203230276,-11.,-51.));
#11427=CARTESIAN_POINT('Origin',(-13.,0.,-55.));
#11428=CARTESIAN_POINT('',(-11.5,-1.83697019872103E-16,-55.));
#11429=CARTESIAN_POINT('Origin',(-13.,0.,-55.));
#11430=CARTESIAN_POINT('',(-11.5,-1.83697019872103E-16,-51.));
#11431=CARTESIAN_POINT('',(-11.5,-1.83697019872103E-16,-55.));
#11432=CARTESIAN_POINT('Origin',(-13.,0.,-51.));
#11433=CARTESIAN_POINT('Origin',(-13.,0.,-51.));
#11434=CARTESIAN_POINT('',(-14.25,0.,-51.));
#11435=CARTESIAN_POINT('Origin',(-13.,0.,-51.));
#11436=CARTESIAN_POINT('Origin',(6.928203230276,11.,-55.));
#11437=CARTESIAN_POINT('',(8.428203230276,11.,-55.));
#11438=CARTESIAN_POINT('Origin',(6.928203230276,11.,-55.));
#11439=CARTESIAN_POINT('',(8.428203230276,11.,-51.));
#11440=CARTESIAN_POINT('',(8.428203230276,11.,-55.));
#11441=CARTESIAN_POINT('Origin',(6.928203230276,11.,-51.));
#11442=CARTESIAN_POINT('Origin',(6.928203230276,11.,-51.));
#11443=CARTESIAN_POINT('',(5.678203230276,11.,-51.));
#11444=CARTESIAN_POINT('Origin',(6.928203230276,11.,-51.));
#11445=CARTESIAN_POINT('Origin',(14.,0.,-22.));
#11446=CARTESIAN_POINT('',(14.,-1.5,-22.));
#11447=CARTESIAN_POINT('Origin',(14.,0.,-22.));
#11448=CARTESIAN_POINT('',(9.,-1.5,-22.));
#11449=CARTESIAN_POINT('',(14.,-1.5,-22.));
#11450=CARTESIAN_POINT('Origin',(9.,0.,-22.));
#11451=CARTESIAN_POINT('Origin',(9.,0.,-22.));
#11452=CARTESIAN_POINT('',(9.,1.25,-22.));
#11453=CARTESIAN_POINT('Origin',(9.,0.,-22.));
#11454=CARTESIAN_POINT('Origin',(49.,0.,-22.));
#11455=CARTESIAN_POINT('',(49.,-1.75,-22.));
#11456=CARTESIAN_POINT('Origin',(49.,0.,-22.));
#11457=CARTESIAN_POINT('',(37.,-1.75,-22.));
#11458=CARTESIAN_POINT('',(49.,-1.75,-22.));
#11459=CARTESIAN_POINT('Origin',(37.,0.,-22.));
#11460=CARTESIAN_POINT('Origin',(37.,0.,-22.));
#11461=CARTESIAN_POINT('',(37.,2.,-22.));
#11462=CARTESIAN_POINT('Origin',(37.,0.,-22.));
#11463=CARTESIAN_POINT('',(0.,0.,0.));
#11464=CARTESIAN_POINT('Origin',(0.,0.,0.));
#11465=CARTESIAN_POINT('',(-16.,0.,1.95943487863577E-15));
#11466=CARTESIAN_POINT('Origin',(0.,0.,0.));
#11467=CARTESIAN_POINT('',(-10.,0.,0.));
#11468=CARTESIAN_POINT('Origin',(0.,0.,0.));
#11469=CARTESIAN_POINT('',(-14.5,0.,0.));
#11470=CARTESIAN_POINT('Origin',(-13.,0.,0.));
#11471=CARTESIAN_POINT('',(5.428203230276,0.,-11.));
#11472=CARTESIAN_POINT('Origin',(6.928203230276,0.,-11.));
#11473=CARTESIAN_POINT('',(5.428203230276,0.,11.));
#11474=CARTESIAN_POINT('Origin',(6.928203230276,0.,11.));
#11475=CARTESIAN_POINT('Origin',(0.,-1.5325,0.));
#11476=CARTESIAN_POINT('',(-10.,-1.,0.));
#11477=CARTESIAN_POINT('',(-10.,-1.5325,1.22464679914735E-15));
#11478=CARTESIAN_POINT('Origin',(0.,-1.,0.));
#11479=CARTESIAN_POINT('Origin',(0.,-1.,0.));
#11480=CARTESIAN_POINT('',(-2.,-1.,0.));
#11481=CARTESIAN_POINT('Origin',(0.,-1.,0.));
#11482=CARTESIAN_POINT('Origin',(0.,-1.5325,0.));
#11483=CARTESIAN_POINT('',(-2.,9.65,0.));
#11484=CARTESIAN_POINT('',(-2.,-1.5325,2.44929359829471E-16));
#11485=CARTESIAN_POINT('Origin',(0.,9.65,0.));
#11486=CARTESIAN_POINT('Origin',(0.,9.65,0.));
#11487=CARTESIAN_POINT('',(-5.99855242977275,9.65,-0.131790543163854));
#11488=CARTESIAN_POINT('Origin',(0.,9.65,0.));
#11489=CARTESIAN_POINT('Origin',(0.,8.65,0.));
#11490=CARTESIAN_POINT('',(-6.99831116806821,8.65,-0.153755633691163));
#11491=CARTESIAN_POINT('Origin',(-5.99855242977275,8.65,-0.131790543163854));
#11492=CARTESIAN_POINT('',(-7.,8.65,0.));
#11493=CARTESIAN_POINT('Origin',(0.,8.65,0.));
#11494=CARTESIAN_POINT('Origin',(0.,8.65,0.));
#11495=CARTESIAN_POINT('Origin',(0.,-1.5325,0.));
#11496=CARTESIAN_POINT('',(-7.,4.,8.57252759403147E-16));
#11497=CARTESIAN_POINT('',(-7.,-1.5325,8.57252759403147E-16));
#11498=CARTESIAN_POINT('Origin',(0.,4.,0.));
#11499=CARTESIAN_POINT('Origin',(0.,4.,0.));
#11500=CARTESIAN_POINT('',(-15.4992842022549,4.,-0.148960456934868));
#11501=CARTESIAN_POINT('Origin',(0.,4.,0.));
#11502=CARTESIAN_POINT('',(-14.5,4.,0.));
#11503=CARTESIAN_POINT('Origin',(-13.,4.,0.));
#11504=CARTESIAN_POINT('',(5.428203230276,4.,-11.));
#11505=CARTESIAN_POINT('Origin',(6.928203230276,4.,-11.));
#11506=CARTESIAN_POINT('',(5.428203230276,4.,11.));
#11507=CARTESIAN_POINT('Origin',(6.928203230276,4.,11.));
#11508=CARTESIAN_POINT('Origin',(-13.,4.,0.));
#11509=CARTESIAN_POINT('',(-14.5,4.,1.83697019872103E-16));
#11510=CARTESIAN_POINT('Origin',(6.928203230276,4.,-11.));
#11511=CARTESIAN_POINT('',(5.428203230276,4.,-11.));
#11512=CARTESIAN_POINT('Origin',(6.928203230276,4.,11.));
#11513=CARTESIAN_POINT('',(5.428203230276,4.,11.));
#11514=CARTESIAN_POINT('Origin',(0.,3.5,0.));
#11515=CARTESIAN_POINT('',(-15.9992611120051,3.5,-0.153765632965025));
#11516=CARTESIAN_POINT('Origin',(-15.4992842022549,3.5,-0.148960456934868));
#11517=CARTESIAN_POINT('',(-16.,3.5,0.));
#11518=CARTESIAN_POINT('Origin',(0.,3.5,0.));
#11519=CARTESIAN_POINT('Origin',(0.,3.5,0.));
#11520=CARTESIAN_POINT('Origin',(0.,-1.5325,0.));
#11521=CARTESIAN_POINT('',(-16.,-1.5325,1.95943487863577E-15));
#11522=CARTESIAN_POINT('',(0.,0.,0.));
#11523=CARTESIAN_POINT('Origin',(2.5,6.35,0.));
#11524=CARTESIAN_POINT('',(2.14860532402759,6.34999974649317,8.70644660934498E-7));
#11525=CARTESIAN_POINT('',(2.8478479312681,6.34999003058963,5.15480744294665E-6));
#11526=CARTESIAN_POINT('Ctrl Pts',(2.1486053225045,6.34999974649289,3.65871305311616E-18));
#11527=CARTESIAN_POINT('Ctrl Pts',(2.14860981858709,6.32558894509038,3.65871305311616E-18));
#11528=CARTESIAN_POINT('Ctrl Pts',(2.1520163214667,6.30133488915141,-3.08118123936608E-14));
#11529=CARTESIAN_POINT('Ctrl Pts',(2.16455445600999,6.25365679968968,-3.08118123936608E-14));
#11530=CARTESIAN_POINT('Ctrl Pts',(2.17377138804027,6.23034157217996,-3.09576802169716E-14));
#11531=CARTESIAN_POINT('Ctrl Pts',(2.20956345199181,6.16111636506853,-3.09576802169716E-14));
#11532=CARTESIAN_POINT('Ctrl Pts',(2.24442612782612,6.11856284402862,-3.22770038253786E-14));
#11533=CARTESIAN_POINT('Ctrl Pts',(2.31888272951377,6.05624332235576,-3.22770038253786E-14));
#11534=CARTESIAN_POINT('Ctrl Pts',(2.35750239145032,6.03309219630646,-3.42413397489756E-14));
#11535=CARTESIAN_POINT('Ctrl Pts',(2.43122237823416,6.00648674167113,-3.42413397489756E-14));
#11536=CARTESIAN_POINT('Ctrl Pts',(2.46540202197458,5.99983772837923,-3.50466365285637E-14));
#11537=CARTESIAN_POINT('Ctrl Pts',(2.53454022793098,6.00026453242939,-3.50466365285637E-14));
#11538=CARTESIAN_POINT('Ctrl Pts',(2.56868396399153,6.00727311231843,-3.43411381866254E-14));
#11539=CARTESIAN_POINT('Ctrl Pts',(2.64251672073783,6.03475210628683,-3.43411381866254E-14));
#11540=CARTESIAN_POINT('Ctrl Pts',(2.68113652459894,6.05843083260967,-3.21032521178046E-14));
#11541=CARTESIAN_POINT('Ctrl Pts',(2.75646506084904,6.12284688425985,-3.21032521178045E-14));
#11542=CARTESIAN_POINT('Ctrl Pts',(2.79073198571329,6.16644333813941,-2.3349794938747E-14));
#11543=CARTESIAN_POINT('Ctrl Pts',(2.82474145767008,6.23412167292725,-2.3349794938747E-14));
#11544=CARTESIAN_POINT('Ctrl Pts',(2.83343278835146,6.2567646493699,-2.41677926809621E-14));
#11545=CARTESIAN_POINT('Ctrl Pts',(2.8451097183543,6.30324581117954,-2.41677926809621E-14));
#11546=CARTESIAN_POINT('Ctrl Pts',(2.84795198077779,6.32630237599366,6.695966560974E-17));
#11547=CARTESIAN_POINT('Ctrl Pts',(2.84784813424439,6.34999165496226,6.695966560974E-17));
#11548=CARTESIAN_POINT('Ctrl Pts',(2.84815123000917,6.34999228813821,-1.05605361430648E-16));
#11549=CARTESIAN_POINT('Ctrl Pts',(2.84815609492309,6.37365275855263,-1.05605361430648E-16));
#11550=CARTESIAN_POINT('Ctrl Pts',(2.84496435783334,6.39716343968712,-1.99114533756745E-14));
#11551=CARTESIAN_POINT('Ctrl Pts',(2.83316209106941,6.44347800850811,-1.99114533756745E-14));
#11552=CARTESIAN_POINT('Ctrl Pts',(2.82446061839549,6.46618019518869,-1.99676121479179E-14));
#11553=CARTESIAN_POINT('Ctrl Pts',(2.78983170226385,6.53526148665337,-1.99676121479179E-14));
#11554=CARTESIAN_POINT('Ctrl Pts',(2.75535086791679,6.5782452428205,-2.11426632102796E-14));
#11555=CARTESIAN_POINT('Ctrl Pts',(2.68122114567467,6.64162093032331,-2.11426632102796E-14));
#11556=CARTESIAN_POINT('Ctrl Pts',(2.64251574891792,6.66533843223839,-2.16999633566802E-14));
#11557=CARTESIAN_POINT('Ctrl Pts',(2.5686604418669,6.69282040482859,-2.16999633566802E-14));
#11558=CARTESIAN_POINT('Ctrl Pts',(2.53453195804941,6.69982796752832,-2.21446346512339E-14));
#11559=CARTESIAN_POINT('Ctrl Pts',(2.46541194722646,6.70025495629189,-2.21446346512339E-14));
#11560=CARTESIAN_POINT('Ctrl Pts',(2.43124007875004,6.69360737099457,-2.18419242653537E-14));
#11561=CARTESIAN_POINT('Ctrl Pts',(2.35752298816286,6.6670078332254,-2.18419242653537E-14));
#11562=CARTESIAN_POINT('Ctrl Pts',(2.31889621664184,6.6438557899457,-2.14275374584633E-14));
#11563=CARTESIAN_POINT('Ctrl Pts',(2.2444310357439,6.58153621615099,-2.14275374584633E-14));
#11564=CARTESIAN_POINT('Ctrl Pts',(2.20956813686693,6.53898582858603,-2.0492122078762E-14));
#11565=CARTESIAN_POINT('Ctrl Pts',(2.1737661560062,6.46974575644438,-2.0492122078762E-14));
#11566=CARTESIAN_POINT('Ctrl Pts',(2.16454384175254,6.44641342304313,-2.02715049049549E-14));
#11567=CARTESIAN_POINT('Ctrl Pts',(2.15200448436394,6.39870188647906,-2.02715049049549E-14));
#11568=CARTESIAN_POINT('Ctrl Pts',(2.14860099263747,6.37442980938693,2.47455274716954E-18));
#11569=CARTESIAN_POINT('Ctrl Pts',(2.14860532218071,6.34999974649284,2.47455274716954E-18));
#11570=CARTESIAN_POINT('Ctrl Pts',(1.965062045595,6.552581420145,-0.9330800615582));
#11571=CARTESIAN_POINT('Ctrl Pts',(2.189120896398,6.506720309034,-0.461213217722));
#11572=CARTESIAN_POINT('Ctrl Pts',(2.281137760944,6.414998086811,0.6484217724168));
#11573=CARTESIAN_POINT('Ctrl Pts',(1.286585694332,6.277414753478,1.992594001388));
#11574=CARTESIAN_POINT('Ctrl Pts',(-0.3475095635628,6.139831420145,2.346140516093));
#11575=CARTESIAN_POINT('Ctrl Pts',(-1.808863355149,6.002248086811,1.534037087326));
#11576=CARTESIAN_POINT('Ctrl Pts',(-2.371417852518,5.864664753478,-0.04036000087055));
#11577=CARTESIAN_POINT('Ctrl Pts',(-1.755619809682,5.727081420145,-1.594692483255));
#11578=CARTESIAN_POINT('Ctrl Pts',(-0.2674627113239,5.589498086811,-2.356631432544));
#11579=CARTESIAN_POINT('Ctrl Pts',(1.353595852992,5.451914753478,-1.947569137845));
#11580=CARTESIAN_POINT('Ctrl Pts',(2.302058075825,5.314331420145,-0.570767882745));
#11581=CARTESIAN_POINT('Ctrl Pts',(2.106637066738,5.176748086811,1.089645653198));
#11582=CARTESIAN_POINT('Ctrl Pts',(0.8644366963533,5.039164753478,2.208618700598));
#11583=CARTESIAN_POINT('Ctrl Pts',(-0.8072987362944,4.901581420145,2.230138139478));
#11584=CARTESIAN_POINT('Ctrl Pts',(-2.077890724405,4.763998086811,1.143511043905));
#11585=CARTESIAN_POINT('Ctrl Pts',(-2.31598729768,4.626414753478,-0.5113220189456));
#11586=CARTESIAN_POINT('Ctrl Pts',(-1.403279241419,4.488831420145,-1.912081258926));
#11587=CARTESIAN_POINT('Ctrl Pts',(0.206712538824,4.351248086811,-2.362735130395));
#11588=CARTESIAN_POINT('Ctrl Pts',(1.713989702755,4.213664753478,-1.639355565149));
#11589=CARTESIAN_POINT('Ctrl Pts',(2.369592383424,4.076081420145,-0.1013869148015));
#11590=CARTESIAN_POINT('Ctrl Pts',(1.847754286391,3.938498086811,1.486960479376));
#11591=CARTESIAN_POINT('Ctrl Pts',(0.4077746306339,3.800914753478,2.336443284436));
#11592=CARTESIAN_POINT('Ctrl Pts',(-1.234826573077,3.663331420145,2.024956962767));
#11593=CARTESIAN_POINT('Ctrl Pts',(-2.263847498087,3.525748086811,0.7072777996607));
#11594=CARTESIAN_POINT('Ctrl Pts',(-2.167971838247,3.388164753478,-0.961844825848));
#11595=CARTESIAN_POINT('Ctrl Pts',(-0.9948398588049,3.250581420145,-2.153030639647));
#11596=CARTESIAN_POINT('Ctrl Pts',(0.6726241054473,3.112998086811,-2.274384493346));
#11597=CARTESIAN_POINT('Ctrl Pts',(2.005863443573,2.975414753478,-1.265605340552));
#11598=CARTESIAN_POINT('Ctrl Pts',(2.342399127393,2.837831420145,0.3720455468077));
#11599=CARTESIAN_POINT('Ctrl Pts',(1.514999911603,2.700248086811,1.824837442277));
#11600=CARTESIAN_POINT('Ctrl Pts',(-0.06517291272752,2.562664753478,2.370841772339));
#11601=CARTESIAN_POINT('Ctrl Pts',(-1.613049883864,2.425081420145,1.738908759939));
#11602=CARTESIAN_POINT('Ctrl Pts',(-2.359079411806,2.287498086811,0.2424553735028));
#11603=CARTESIAN_POINT('Ctrl Pts',(-2.075774396281,2.195775864589,-0.8343432069565));
#11604=CARTESIAN_POINT('Ctrl Pts',(-1.773180685345,2.149914753478,-1.260133922024));
#11605=CARTESIAN_POINT('Ctrl Pts',(1.950430605956,6.514669866795,-0.9261325432193));
#11606=CARTESIAN_POINT('Ctrl Pts',(2.172821161573,6.468808755684,-0.4577791208848));
#11607=CARTESIAN_POINT('Ctrl Pts',(2.264152887855,6.377086533461,0.6435937599656));
#11608=CARTESIAN_POINT('Ctrl Pts',(1.277006047232,6.239503200128,1.977757564583));
#11609=CARTESIAN_POINT('Ctrl Pts',(-0.3449220802747,6.101919866795,2.328671646129));
#11610=CARTESIAN_POINT('Ctrl Pts',(-1.795394938182,5.964336533461,1.522614969079));
#11611=CARTESIAN_POINT('Ctrl Pts',(-2.353760772811,5.826753200128,-0.04005948877329));
#11612=CARTESIAN_POINT('Ctrl Pts',(-1.742547832982,5.689169866795,-1.582818737658));
#11613=CARTESIAN_POINT('Ctrl Pts',(-0.2654712401003,5.551586533461,-2.339084449417));
#11614=CARTESIAN_POINT('Ctrl Pts',(1.343517262312,5.414003200128,-1.933067946727));
#11615=CARTESIAN_POINT('Ctrl Pts',(2.284917434461,5.276419866795,-0.5665180648611));
#11616=CARTESIAN_POINT('Ctrl Pts',(2.0909514892,5.138836533461,1.081532380318));
#11617=CARTESIAN_POINT('Ctrl Pts',(0.8580002821075,5.001253200128,2.192173789215));
#11618=CARTESIAN_POINT('Ctrl Pts',(-0.8012877593092,4.863669866795,2.213532998868));
#11619=CARTESIAN_POINT('Ctrl Pts',(-2.0624191861,4.726086533461,1.134996700628));
#11620=CARTESIAN_POINT('Ctrl Pts',(-2.298742942253,4.588503200128,-0.5075148224894));
#11621=CARTESIAN_POINT('Ctrl Pts',(-1.392830718655,4.450919866795,-1.897844303107));
#11622=CARTESIAN_POINT('Ctrl Pts',(0.2051734006369,4.313336533461,-2.345142700415));
#11623=CARTESIAN_POINT('Ctrl Pts',(1.701227695095,4.175753200128,-1.627149267617));
#11624=CARTESIAN_POINT('Ctrl Pts',(2.351948895778,4.038169866795,-0.1006320091092));
#11625=CARTESIAN_POINT('Ctrl Pts',(1.833996295711,3.900586533461,1.475888883674));
#11626=CARTESIAN_POINT('Ctrl Pts',(0.4047384263025,3.763003200128,2.319046618024));
#11627=CARTESIAN_POINT('Ctrl Pts',(-1.225632313532,3.625419866795,2.009879558143));
#11628=CARTESIAN_POINT('Ctrl Pts',(-2.246991364667,3.487836533461,0.7020115575811));
#11629=CARTESIAN_POINT('Ctrl Pts',(-2.151829574871,3.350253200128,-0.9546831311102));
#11630=CARTESIAN_POINT('Ctrl Pts',(-0.9874324899755,3.212669866795,-2.1369996253));
#11631=CARTESIAN_POINT('Ctrl Pts',(0.6676158875029,3.075086533461,-2.25744990367));
#11632=CARTESIAN_POINT('Ctrl Pts',(1.990928205287,2.937503200128,-1.256181908764));
#11633=CARTESIAN_POINT('Ctrl Pts',(2.324958115024,2.799919866795,0.3692753737369));
#11634=CARTESIAN_POINT('Ctrl Pts',(1.503719540172,2.662336533461,1.811250085609));
#11635=CARTESIAN_POINT('Ctrl Pts',(-0.06468764889537,2.524753200128,2.353188982004));
#11636=CARTESIAN_POINT('Ctrl Pts',(-1.601039452915,2.387169866795,1.725961210209));
#11637=CARTESIAN_POINT('Ctrl Pts',(-2.34151420154,2.249586533461,0.2406501016691));
#11638=CARTESIAN_POINT('Ctrl Pts',(-2.060318615711,2.157864311239,-0.8281308625178));
#11639=CARTESIAN_POINT('Ctrl Pts',(-1.759977954049,2.112003200128,-1.250751229269));
#11640=CARTESIAN_POINT('Ctrl Pts',(1.924102649941,6.387168266731,-0.9136311105677));
#11641=CARTESIAN_POINT('Ctrl Pts',(2.143491258835,6.34130715562,-0.4515997733487));
#11642=CARTESIAN_POINT('Ctrl Pts',(2.233590140603,6.249584933397,0.6349061869998));
#11643=CARTESIAN_POINT('Ctrl Pts',(1.259768336267,6.112001600064,1.951060734658));
#11644=CARTESIAN_POINT('Ctrl Pts',(-0.3402661374637,5.974418266731,2.297237990153));
#11645=CARTESIAN_POINT('Ctrl Pts',(-1.771159736572,5.836834933397,1.502061897459));
#11646=CARTESIAN_POINT('Ctrl Pts',(-2.321988450378,5.699251600064,-0.03951874435758));
#11647=CARTESIAN_POINT('Ctrl Pts',(-1.719025989877,5.561668266731,-1.561453003354));
#11648=CARTESIAN_POINT('Ctrl Pts',(-0.261887767245,5.424084933397,-2.307510235851));
#11649=CARTESIAN_POINT('Ctrl Pts',(1.325381747376,5.286501600064,-1.906974361177));
#11650=CARTESIAN_POINT('Ctrl Pts',(2.254074396247,5.148918266731,-0.5588709008719));
#11651=CARTESIAN_POINT('Ctrl Pts',(2.062726707109,5.011334933397,1.066933277509));
#11652=CARTESIAN_POINT('Ctrl Pts',(0.8464185351747,4.873751600064,2.162582654353));
#11653=CARTESIAN_POINT('Ctrl Pts',(-0.7904715483566,4.736168266731,2.183653545964));
#11654=CARTESIAN_POINT('Ctrl Pts',(-2.034579548304,4.598584933397,1.119675907815));
#11655=CARTESIAN_POINT('Ctrl Pts',(-2.267713279938,4.461001600064,-0.500664115839));
#11656=CARTESIAN_POINT('Ctrl Pts',(-1.374029544296,4.323418266731,-1.872226185147));
#11657=CARTESIAN_POINT('Ctrl Pts',(0.2024038602847,4.185834933397,-2.313486709334));
#11658=CARTESIAN_POINT('Ctrl Pts',(1.678263613322,4.048251600064,-1.605185136098));
#11659=CARTESIAN_POINT('Ctrl Pts',(2.32020103103,3.910668266731,-0.09927362440098));
#11660=CARTESIAN_POINT('Ctrl Pts',(1.809240032321,3.773084933397,1.455966545758));
#11661=CARTESIAN_POINT('Ctrl Pts',(0.3992750504445,3.635501600064,2.287742885828));
#11662=CARTESIAN_POINT('Ctrl Pts',(-1.209088072716,3.497918266731,1.98274912836));
#11663=CARTESIAN_POINT('Ctrl Pts',(-2.216660272838,3.360334933397,0.6925354299232));
#11664=CARTESIAN_POINT('Ctrl Pts',(-2.122783027803,3.222751600064,-0.9417963073456));
#11665=CARTESIAN_POINT('Ctrl Pts',(-0.9741035978403,3.085168266731,-2.108153260827));
#11666=CARTESIAN_POINT('Ctrl Pts',(0.6586040510052,2.947584933397,-2.226977636885));
#11667=CARTESIAN_POINT('Ctrl Pts',(1.964053591005,2.810001600064,-1.239225293163));
#11668=CARTESIAN_POINT('Ctrl Pts',(2.293574586278,2.672418266731,0.3642906971391));
#11669=CARTESIAN_POINT('Ctrl Pts',(1.483421529162,2.534834933397,1.786800862735));
#11670=CARTESIAN_POINT('Ctrl Pts',(-0.06381446039555,2.397251600064,2.321424377909));
#11671=CARTESIAN_POINT('Ctrl Pts',(-1.579427765646,2.259668266731,1.702663262213));
#11672=CARTESIAN_POINT('Ctrl Pts',(-2.309907189879,2.122084933397,0.2374016778224));
#11673=CARTESIAN_POINT('Ctrl Pts',(-2.032507332538,2.030362711175,-0.8169523089941));
#11674=CARTESIAN_POINT('Ctrl Pts',(-1.736220829843,1.984501600064,-1.233867919887));
#11675=CARTESIAN_POINT('Ctrl Pts',(2.02121917785,6.172166666667,-0.9597454284554));
#11676=CARTESIAN_POINT('Ctrl Pts',(2.251681135642,6.126305555556,-0.4743936726209));
#11677=CARTESIAN_POINT('Ctrl Pts',(2.346327638903,6.034583333333,0.6669522342475));
#11678=CARTESIAN_POINT('Ctrl Pts',(1.323353471287,5.897,2.049537936119));
#11679=CARTESIAN_POINT('Ctrl Pts',(-0.357440619208,5.759416666667,2.413188029197));
#11680=CARTESIAN_POINT('Ctrl Pts',(-1.860556673889,5.621833333333,1.577876478448));
#11681=CARTESIAN_POINT('Ctrl Pts',(-2.439187736057,5.48425,-0.04151340053637));
#11682=CARTESIAN_POINT('Ctrl Pts',(-1.805791545513,5.346666666667,-1.6402652716));
#11683=CARTESIAN_POINT('Ctrl Pts',(-0.2751062047631,5.209083333333,-2.423978752864));
#11684=CARTESIAN_POINT('Ctrl Pts',(1.39227863225,5.0715,-2.00322636144));
#11685=CARTESIAN_POINT('Ctrl Pts',(2.367845810168,4.933916666667,-0.5870791679536));
#11686=CARTESIAN_POINT('Ctrl Pts',(2.166840100345,4.796333333333,1.120785318836));
#11687=CARTESIAN_POINT('Ctrl Pts',(0.8891403875127,4.65875,2.271736144014));
#11688=CARTESIAN_POINT('Ctrl Pts',(-0.8303695507784,4.521166666667,2.293870560918));
#11689=CARTESIAN_POINT('Ctrl Pts',(-2.137272251052,4.383583333333,1.176190063415));
#11690=CARTESIAN_POINT('Ctrl Pts',(-2.382173098413,4.246,-0.5259344726884));
#11691=CARTESIAN_POINT('Ctrl Pts',(-1.443381862163,4.108416666667,-1.966724317338));
#11692=CARTESIAN_POINT('Ctrl Pts',(0.212619926536,3.970833333333,-2.430256880916));
#11693=CARTESIAN_POINT('Ctrl Pts',(1.762971742094,3.83325,-1.68620472571));
#11694=CARTESIAN_POINT('Ctrl Pts',(2.437310099089,3.695666666667,-0.1042843288533));
#11695=CARTESIAN_POINT('Ctrl Pts',(1.900559022032,3.558083333333,1.529454525041));
#11696=CARTESIAN_POINT('Ctrl Pts',(0.4194279287647,3.4205,2.403213672081));
#11697=CARTESIAN_POINT('Ctrl Pts',(-1.270115188687,3.282916666667,2.082825759441));
#11698=CARTESIAN_POINT('Ctrl Pts',(-2.328543258529,3.145333333333,0.7274902367315));
#11699=CARTESIAN_POINT('Ctrl Pts',(-2.229927684129,3.00775,-0.9893322261645));
#11700=CARTESIAN_POINT('Ctrl Pts',(-1.023270184274,2.870166666667,-2.21455949908));
#11701=CARTESIAN_POINT('Ctrl Pts',(0.6918462164907,2.732583333333,-2.339381377835));
#11702=CARTESIAN_POINT('Ctrl Pts',(2.063186589648,2.595,-1.301773545343));
#11703=CARTESIAN_POINT('Ctrl Pts',(2.409339719873,2.457416666667,0.3826777866516));
#11704=CARTESIAN_POINT('Ctrl Pts',(1.558295262298,2.319833333333,1.876987265138));
#11705=CARTESIAN_POINT('Ctrl Pts',(-0.06703541060015,2.18225,2.438595192779));
#11706=CARTESIAN_POINT('Ctrl Pts',(-1.659147286165,2.044666666667,1.788602930884));
#11707=CARTESIAN_POINT('Ctrl Pts',(-2.426496689966,1.907083333333,0.2493842124707));
#11708=CARTESIAN_POINT('Ctrl Pts',(-2.135095442945,1.815361111111,-0.8581868926683));
#11709=CARTESIAN_POINT('Ctrl Pts',(-1.823854272208,1.7695,-1.29614576576));
#11710=CARTESIAN_POINT('Ctrl Pts',(2.22783143602,6.057791466659,-1.057852141678));
#11711=CARTESIAN_POINT('Ctrl Pts',(2.481851583861,6.011930355548,-0.5228869528331));
#11712=CARTESIAN_POINT('Ctrl Pts',(2.586173004113,5.920208133325,0.7351291587096));
#11713=CARTESIAN_POINT('Ctrl Pts',(1.458628780396,5.782624799992,2.259044983067));
#11714=CARTESIAN_POINT('Ctrl Pts',(-0.3939787711836,5.645041466659,2.659867970475));
#11715=CARTESIAN_POINT('Ctrl Pts',(-2.050745753855,5.507458133325,1.739169536568));
#11716=CARTESIAN_POINT('Ctrl Pts',(-2.688525408967,5.369874799992,-0.04575696675776));
#11717=CARTESIAN_POINT('Ctrl Pts',(-1.990382446436,5.232291466659,-1.807935811973));
#11718=CARTESIAN_POINT('Ctrl Pts',(-0.3032280011649,5.094708133325,-2.67176173918));
#11719=CARTESIAN_POINT('Ctrl Pts',(1.534599581587,4.957124799992,-2.20799936513));
#11720=CARTESIAN_POINT('Ctrl Pts',(2.609890797272,4.819541466659,-0.6470913397877));
#11721=CARTESIAN_POINT('Ctrl Pts',(2.388337962196,4.681958133325,1.235353787306));
#11722=CARTESIAN_POINT('Ctrl Pts',(0.9800297404872,4.544374799992,2.503956647275));
#11723=CARTESIAN_POINT('Ctrl Pts',(-0.9152512547927,4.406791466659,2.528353679688));
#11724=CARTESIAN_POINT('Ctrl Pts',(-2.355747640042,4.269208133325,1.29642209352));
#11725=CARTESIAN_POINT('Ctrl Pts',(-2.625682643845,4.131624799992,-0.5796963359453));
#11726=CARTESIAN_POINT('Ctrl Pts',(-1.590926665424,3.994041466659,-2.167766023679));
#11727=CARTESIAN_POINT('Ctrl Pts',(0.2343542756037,3.856458133325,-2.678681627526));
#11728=CARTESIAN_POINT('Ctrl Pts',(1.943185534203,3.718874799992,-1.858571270583));
#11729=CARTESIAN_POINT('Ctrl Pts',(2.686455836945,3.581291466659,-0.1149444397964));
#11730=CARTESIAN_POINT('Ctrl Pts',(2.094837206026,3.443708133325,1.685797813611));
#11731=CARTESIAN_POINT('Ctrl Pts',(0.4623025226986,3.306124799992,2.648874018616));
#11732=CARTESIAN_POINT('Ctrl Pts',(-1.399948395371,3.168541466659,2.295735540948));
#11733=CARTESIAN_POINT('Ctrl Pts',(-2.566570675924,3.030958133325,0.8018554526641));
#11734=CARTESIAN_POINT('Ctrl Pts',(-2.457874459731,2.893374799992,-1.090463349186));
#11735=CARTESIAN_POINT('Ctrl Pts',(-1.127870499672,2.755791466659,-2.440935314217));
#11736=CARTESIAN_POINT('Ctrl Pts',(0.7625678436463,2.618208133325,-2.578516685126));
#11737=CARTESIAN_POINT('Ctrl Pts',(2.274088823798,2.480624799992,-1.434842919896));
#11738=CARTESIAN_POINT('Ctrl Pts',(2.655626280814,2.343041466659,0.4217957222611));
#11739=CARTESIAN_POINT('Ctrl Pts',(1.717586697175,2.205458133325,2.06885590643));
#11740=CARTESIAN_POINT('Ctrl Pts',(-0.07388787752371,2.067874799992,2.687872294968));
#11741=CARTESIAN_POINT('Ctrl Pts',(-1.828747976278,1.930291466659,1.97143678412));
#11742=CARTESIAN_POINT('Ctrl Pts',(-2.674537063841,1.792708133325,0.2748766656669));
#11743=CARTESIAN_POINT('Ctrl Pts',(-2.353348315127,1.700985911103,-0.9459121298763));
#11744=CARTESIAN_POINT('Ctrl Pts',(-2.010291573953,1.655124799992,-1.428639859679));
#11745=CARTESIAN_POINT('Ctrl Pts',(2.404044642027,6.11768501526,-1.141524323672));
#11746=CARTESIAN_POINT('Ctrl Pts',(2.678156841681,6.071823904148,-0.5642453719883));
#11747=CARTESIAN_POINT('Ctrl Pts',(2.790729699461,5.980101681926,0.7932751493761));
#11748=CARTESIAN_POINT('Ctrl Pts',(1.574000908471,5.842518348593,2.437727064909));
#11749=CARTESIAN_POINT('Ctrl Pts',(-0.4251410311493,5.70493501526,2.870253664408));
#11750=CARTESIAN_POINT('Ctrl Pts',(-2.21295213902,5.567351681926,1.87673139824));
#11751=CARTESIAN_POINT('Ctrl Pts',(-2.901177800026,5.429768348593,-0.04937617316592));
#11752=CARTESIAN_POINT('Ctrl Pts',(-2.147814317805,5.29218501526,-1.95093683105));
#11753=CARTESIAN_POINT('Ctrl Pts',(-0.3272122117171,5.154601681926,-2.883088186116));
#11754=CARTESIAN_POINT('Ctrl Pts',(1.655980718345,5.017018348593,-2.382643927865));
#11755=CARTESIAN_POINT('Ctrl Pts',(2.816323482115,4.87943501526,-0.6982738654132));
#11756=CARTESIAN_POINT('Ctrl Pts',(2.577246639281,4.741851681926,1.333065691311));
#11757=CARTESIAN_POINT('Ctrl Pts',(1.057546459105,4.604268348593,2.702010333647));
#11758=CARTESIAN_POINT('Ctrl Pts',(-0.9876442353842,4.46668501526,2.728337080863));
#11759=CARTESIAN_POINT('Ctrl Pts',(-2.542078543486,4.329101681926,1.398964274111));
#11760=CARTESIAN_POINT('Ctrl Pts',(-2.833364405197,4.191518348593,-0.625548166661));
#11761=CARTESIAN_POINT('Ctrl Pts',(-1.716763065658,4.05393501526,-2.339228278286));
#11762=CARTESIAN_POINT('Ctrl Pts',(0.2528908298411,3.916351681926,-2.890555411972));
#11763=CARTESIAN_POINT('Ctrl Pts',(2.096884304816,3.778768348593,-2.005577366684));
#11764=CARTESIAN_POINT('Ctrl Pts',(2.898944532531,3.64118501526,-0.1240361187815));
#11765=CARTESIAN_POINT('Ctrl Pts',(2.260531061571,3.503601681926,1.819138169894));
#11766=CARTESIAN_POINT('Ctrl Pts',(0.4988689380713,3.366018348593,2.858390131722));
#11767=CARTESIAN_POINT('Ctrl Pts',(-1.510679122572,3.22843501526,2.477319709873));
#11768=CARTESIAN_POINT('Ctrl Pts',(-2.769576899795,3.090851681926,0.8652792457679));
#11769=CARTESIAN_POINT('Ctrl Pts',(-2.652283215936,2.953268348593,-1.176714956775));
#11770=CARTESIAN_POINT('Ctrl Pts',(-1.217080874162,2.81568501526,-2.634004246821));
#11771=CARTESIAN_POINT('Ctrl Pts',(0.8228841325514,2.678101681926,-2.78246779403));
#11772=CARTESIAN_POINT('Ctrl Pts',(2.45396081766,2.540518348593,-1.548333674601));
#11773=CARTESIAN_POINT('Ctrl Pts',(2.865676472823,2.40293501526,0.4551581999144));
#11774=CARTESIAN_POINT('Ctrl Pts',(1.853441436277,2.265351681926,2.232494737513));
#11775=CARTESIAN_POINT('Ctrl Pts',(-0.07973213466677,2.127768348593,2.900473027131));
#11776=CARTESIAN_POINT('Ctrl Pts',(-1.973395160382,1.99018501526,2.127370123848));
#11777=CARTESIAN_POINT('Ctrl Pts',(-2.886083028668,1.852601681926,0.2966183907052));
#11778=CARTESIAN_POINT('Ctrl Pts',(-2.539489440867,1.760879459704,-1.020730271999));
#11779=CARTESIAN_POINT('Ctrl Pts',(-2.169298183488,1.715018348593,-1.541639975322));
#11780=CARTESIAN_POINT('Ctrl Pts',(2.522021513594,6.235843307732,-1.197543860985));
#11781=CARTESIAN_POINT('Ctrl Pts',(2.809585584818,6.189982196621,-0.5919353335721));
#11782=CARTESIAN_POINT('Ctrl Pts',(2.92768287977,6.098259974399,0.8322045930226));
#11783=CARTESIAN_POINT('Ctrl Pts',(1.651243942889,5.960676641066,2.557356878692));
#11784=CARTESIAN_POINT('Ctrl Pts',(-0.4460045408999,5.823093307732,3.011109429734));
#11785=CARTESIAN_POINT('Ctrl Pts',(-2.321551274712,5.685509974399,1.968830727539));
#11786=CARTESIAN_POINT('Ctrl Pts',(-3.043551146479,5.547926641066,-0.0517992756068));
#11787=CARTESIAN_POINT('Ctrl Pts',(-2.253216858794,5.410343307732,-2.046677741984));
#11788=CARTESIAN_POINT('Ctrl Pts',(-0.3432699306139,5.272759974399,-3.024573796951));
#11789=CARTESIAN_POINT('Ctrl Pts',(1.737246856715,5.135176641066,-2.499570573799));
#11790=CARTESIAN_POINT('Ctrl Pts',(2.95453266007,4.997593307732,-0.7325411850372));
#11791=CARTESIAN_POINT('Ctrl Pts',(2.703723282204,4.860009974399,1.398484992228));
#11792=CARTESIAN_POINT('Ctrl Pts',(1.109444839277,4.722426641066,2.834609670836));
#11793=CARTESIAN_POINT('Ctrl Pts',(-1.03611221101,4.584843307732,2.862228385439));
#11794=CARTESIAN_POINT('Ctrl Pts',(-2.666829335795,4.447259974399,1.467617503593));
#11795=CARTESIAN_POINT('Ctrl Pts',(-2.972409854974,4.309676641066,-0.6562465216029));
#11796=CARTESIAN_POINT('Ctrl Pts',(-1.801012056782,4.172093307732,-2.45402433046));
#11797=CARTESIAN_POINT('Ctrl Pts',(0.2653012769813,4.034509974399,-3.032407471886));
#11798=CARTESIAN_POINT('Ctrl Pts',(2.199787489722,3.896926641066,-2.103999725101));
#11799=CARTESIAN_POINT('Ctrl Pts',(3.041208282885,3.759343307732,-0.1301231077663));
#11800=CARTESIAN_POINT('Ctrl Pts',(2.37146510084,3.621759974399,1.908411150304));
#11801=CARTESIAN_POINT('Ctrl Pts',(0.5233505951948,3.484176641066,2.998663702172));
#11802=CARTESIAN_POINT('Ctrl Pts',(-1.584814682997,3.346593307732,2.59889250604));
#11803=CARTESIAN_POINT('Ctrl Pts',(-2.905492020709,3.209009974399,0.9077422419465));
#11804=CARTESIAN_POINT('Ctrl Pts',(-2.782442228317,3.071426641066,-1.234461450704));
#11805=CARTESIAN_POINT('Ctrl Pts',(-1.276808298299,2.933843307732,-2.763266231105));
#11806=CARTESIAN_POINT('Ctrl Pts',(0.8632666171041,2.796259974399,-2.919015526896));
#11807=CARTESIAN_POINT('Ctrl Pts',(2.574387291926,2.658676641066,-1.624317106805));
#11808=CARTESIAN_POINT('Ctrl Pts',(3.006307615555,2.521093307732,0.4774947820042));
#11809=CARTESIAN_POINT('Ctrl Pts',(1.94439782638,2.383509974399,2.342052913063));
#11810=CARTESIAN_POINT('Ctrl Pts',(-0.0836449354721,2.245926641066,3.042811787328));
#11811=CARTESIAN_POINT('Ctrl Pts',(-2.0702381987,2.108343307732,2.231769379789));
#11812=CARTESIAN_POINT('Ctrl Pts',(-3.027715609383,1.970759974399,0.3111747384423));
#11813=CARTESIAN_POINT('Ctrl Pts',(-2.664113174709,1.879037752177,-1.070821922587));
#11814=CARTESIAN_POINT('Ctrl Pts',(-2.275755030715,1.833176641066,-1.617294918742));
#11815=CARTESIAN_POINT('Ctrl Pts',(2.585998917206,6.392208093593,-1.227922565736));
#11816=CARTESIAN_POINT('Ctrl Pts',(2.880857772614,6.346346982481,-0.6069512585133));
#11817=CARTESIAN_POINT('Ctrl Pts',(3.001950901767,6.254624760259,0.8533155505813));
#11818=CARTESIAN_POINT('Ctrl Pts',(1.693131888581,6.117041426926,2.622230652499));
#11819=CARTESIAN_POINT('Ctrl Pts',(-0.4573185651349,5.979458093593,3.087493775493));
#11820=CARTESIAN_POINT('Ctrl Pts',(-2.380443247722,5.841874760259,2.01877505887));
#11821=CARTESIAN_POINT('Ctrl Pts',(-3.120758457782,5.704291426926,-0.05311329420039));
#11822=CARTESIAN_POINT('Ctrl Pts',(-2.310375357889,5.566708093593,-2.09859685816));
#11823=CARTESIAN_POINT('Ctrl Pts',(-0.351977833691,5.429124760259,-3.101299700167));
#11824=CARTESIAN_POINT('Ctrl Pts',(1.781316482103,5.291541426926,-2.562978452993));
#11825=CARTESIAN_POINT('Ctrl Pts',(3.029481794112,5.153958093593,-0.7511239301902));
#11826=CARTESIAN_POINT('Ctrl Pts',(2.772310007078,5.016374760259,1.433961072947));
#11827=CARTESIAN_POINT('Ctrl Pts',(1.137588691296,4.878791426926,2.906516657361));
#11828=CARTESIAN_POINT('Ctrl Pts',(-1.062395796916,4.741208093593,2.934835989957));
#11829=CARTESIAN_POINT('Ctrl Pts',(-2.734480153149,4.603624760259,1.504847303921));
#11830=CARTESIAN_POINT('Ctrl Pts',(-3.04781248892,4.466041426926,-0.6728938611896));
#11831=CARTESIAN_POINT('Ctrl Pts',(-1.846699246461,4.328458093593,-2.516276814912));
#11832=CARTESIAN_POINT('Ctrl Pts',(0.2720313095305,4.190874760259,-3.109332095922));
#11833=CARTESIAN_POINT('Ctrl Pts',(2.255590618812,4.053291426926,-2.157372957203));
#11834=CARTESIAN_POINT('Ctrl Pts',(3.118356161574,3.915708093593,-0.1334240068824));
#11835=CARTESIAN_POINT('Ctrl Pts',(2.431623263287,3.778124760259,1.956822787462));
#11836=CARTESIAN_POINT('Ctrl Pts',(0.5366266961634,3.640541426926,3.074732330824));
#11837=CARTESIAN_POINT('Ctrl Pts',(-1.625017483837,3.502958093593,2.66481993525));
#11838=CARTESIAN_POINT('Ctrl Pts',(-2.979197115887,3.365374760259,0.9307694014992));
#11839=CARTESIAN_POINT('Ctrl Pts',(-2.853025856771,3.227791426926,-1.265776662747));
#11840=CARTESIAN_POINT('Ctrl Pts',(-1.309197744382,3.090208093593,-2.833363412276));
#11841=CARTESIAN_POINT('Ctrl Pts',(0.8851655408403,2.952624760259,-2.99306367974));
#11842=CARTESIAN_POINT('Ctrl Pts',(2.639693084894,2.815041426926,-1.665521985739));
#11843=CARTESIAN_POINT('Ctrl Pts',(3.08257015125,2.677458093593,0.4896076352159));
#11844=CARTESIAN_POINT('Ctrl Pts',(1.99372235587,2.539874760259,2.401464961569));
#11845=CARTESIAN_POINT('Ctrl Pts',(-0.08576679913106,2.402291426926,3.120000342931));
#11846=CARTESIAN_POINT('Ctrl Pts',(-2.122754984976,2.264708093593,2.288383809765));
#11847=CARTESIAN_POINT('Ctrl Pts',(-3.104521212555,2.127124760259,0.319068466441));
#11848=CARTESIAN_POINT('Ctrl Pts',(-2.731695089822,2.035402538037,-1.097986007416));
#11849=CARTESIAN_POINT('Ctrl Pts',(-2.33348526709,1.989541426926,-1.658321662257));
#11850=CARTESIAN_POINT('Ctrl Pts',(2.571274775611,6.501639428961,-1.220931029272));
#11851=CARTESIAN_POINT('Ctrl Pts',(2.864454765839,6.45577831785,-0.6034954039063));
#11852=CARTESIAN_POINT('Ctrl Pts',(2.984858415824,6.364056095628,0.848456948782));
#11853=CARTESIAN_POINT('Ctrl Pts',(1.6834915467,6.226472762294,2.607300214916));
#11854=CARTESIAN_POINT('Ctrl Pts',(-0.4547146880558,6.088889428961,3.069914226166));
#11855=CARTESIAN_POINT('Ctrl Pts',(-2.366889497484,5.951306095628,2.007280572303));
#11856=CARTESIAN_POINT('Ctrl Pts',(-3.102989506252,5.813722762294,-0.05281087811692));
#11857=CARTESIAN_POINT('Ctrl Pts',(-2.297220559686,5.676139428961,-2.08664788282));
#11858=CARTESIAN_POINT('Ctrl Pts',(-0.349973744893,5.538556095628,-3.083641542768));
#11859=CARTESIAN_POINT('Ctrl Pts',(1.771174035433,5.400972762294,-2.548385385147));
#11860=CARTESIAN_POINT('Ctrl Pts',(3.012232552977,5.263389428961,-0.7468471862867));
#11861=CARTESIAN_POINT('Ctrl Pts',(2.756525048771,5.125806095628,1.425796395948));
#11862=CARTESIAN_POINT('Ctrl Pts',(1.131111497181,4.988222762294,2.889967554217));
#11863=CARTESIAN_POINT('Ctrl Pts',(-1.05634673555,4.850639428961,2.918125642405));
#11864=CARTESIAN_POINT('Ctrl Pts',(-2.718910590186,4.713056095628,1.496279015422));
#11865=CARTESIAN_POINT('Ctrl Pts',(-3.03045887661,4.575472762294,-0.6690625430769));
#11866=CARTESIAN_POINT('Ctrl Pts',(-1.836184523888,4.437889428961,-2.50194965651));
#11867=CARTESIAN_POINT('Ctrl Pts',(0.2704824196632,4.300306095628,-3.091628203727));
#11868=CARTESIAN_POINT('Ctrl Pts',(2.242747753553,4.162722762294,-2.145089322943));
#11869=CARTESIAN_POINT('Ctrl Pts',(3.100600888221,4.025139428961,-0.1326643182543));
#11870=CARTESIAN_POINT('Ctrl Pts',(2.417778104653,3.887556095628,1.945681044282));
#11871=CARTESIAN_POINT('Ctrl Pts',(0.5335712550317,3.749972762294,3.057225442517));
#11872=CARTESIAN_POINT('Ctrl Pts',(-1.615764971251,3.612389428961,2.649647003123));
#11873=CARTESIAN_POINT('Ctrl Pts',(-2.962234185283,3.474806095628,0.9254697935337));
#11874=CARTESIAN_POINT('Ctrl Pts',(-2.836781319153,3.337222762294,-1.258569592904));
#11875=CARTESIAN_POINT('Ctrl Pts',(-1.301743443904,3.199639428961,-2.81723082854));
#11876=CARTESIAN_POINT('Ctrl Pts',(0.880125591801,3.062056095628,-2.976021795796));
#11877=CARTESIAN_POINT('Ctrl Pts',(2.624663219842,2.924472762294,-1.656038848919));
#11878=CARTESIAN_POINT('Ctrl Pts',(3.065018636018,2.786889428961,0.4868199108673));
#11879=CARTESIAN_POINT('Ctrl Pts',(1.982370514199,2.649306095628,2.387791518052));
#11880=CARTESIAN_POINT('Ctrl Pts',(-0.08527846076163,2.511722762294,3.10223570795));
#11881=CARTESIAN_POINT('Ctrl Pts',(-2.110668458271,2.374139428961,2.275354226878));
#11882=CARTESIAN_POINT('Ctrl Pts',(-3.086844712532,2.236556095628,0.3172517567559));
#11883=CARTESIAN_POINT('Ctrl Pts',(-2.716141384432,2.144833873405,-1.091734302771));
#11884=CARTESIAN_POINT('Ctrl Pts',(-2.320198885857,2.098972762294,-1.648879522586));
#11885=CARTESIAN_POINT('Ctrl Pts',(2.551614418722,6.552581420145,-1.211595605458));
#11886=CARTESIAN_POINT('Ctrl Pts',(2.842552710281,6.506720309034,-0.598880986523));
#11887=CARTESIAN_POINT('Ctrl Pts',(2.962035735699,6.414998086811,0.8419695182762));
#11888=CARTESIAN_POINT('Ctrl Pts',(1.670619315018,6.277414753478,2.587364402054));
#11889=CARTESIAN_POINT('Ctrl Pts',(-0.4512378705897,6.139831420145,3.046441196415));
#11890=CARTESIAN_POINT('Ctrl Pts',(-2.348791901428,6.002248086811,1.991932600627));
#11891=CARTESIAN_POINT('Ctrl Pts',(-3.079263577893,5.864664753478,-0.05240707813364));
#11892=CARTESIAN_POINT('Ctrl Pts',(-2.279655662895,5.727081420145,-2.07069305665));
#11893=CARTESIAN_POINT('Ctrl Pts',(-0.3472977925631,5.589498086811,-3.060063551872));
#11894=CARTESIAN_POINT('Ctrl Pts',(1.757631370145,5.451914753478,-2.528900044009));
#11895=CARTESIAN_POINT('Ctrl Pts',(2.989200566047,5.314331420145,-0.7411366794348));
#11896=CARTESIAN_POINT('Ctrl Pts',(2.735448240199,5.176748086811,1.414894540471));
#11897=CARTESIAN_POINT('Ctrl Pts',(1.122462847131,5.039164753478,2.86787042401));
#11898=CARTESIAN_POINT('Ctrl Pts',(-1.048269748206,4.901581420145,2.895813211186));
#11899=CARTESIAN_POINT('Ctrl Pts',(-2.698121387469,4.763998086811,1.484838239147));
#11900=CARTESIAN_POINT('Ctrl Pts',(-3.007287528446,4.626414753478,-0.6639467894038));
#11901=CARTESIAN_POINT('Ctrl Pts',(-1.822144778546,4.488831420145,-2.482819369995));
#11902=CARTESIAN_POINT('Ctrl Pts',(0.2684142700615,4.351248086811,-3.067989145611));
#11903=CARTESIAN_POINT('Ctrl Pts',(2.225599364098,4.213664753478,-2.12868764466));
#11904=CARTESIAN_POINT('Ctrl Pts',(3.076893223598,4.076081420145,-0.1316499467573));
#11905=CARTESIAN_POINT('Ctrl Pts',(2.399291406589,3.938498086811,1.930804071939));
#11906=CARTESIAN_POINT('Ctrl Pts',(0.5294914882953,3.800914753478,3.03384943313));
#11907=CARTESIAN_POINT('Ctrl Pts',(-1.603410587237,3.663331420145,2.629387400296));
#11908=CARTESIAN_POINT('Ctrl Pts',(-2.939584493455,3.525748086811,0.9183935111373));
#11909=CARTESIAN_POINT('Ctrl Pts',(-2.815090858966,3.388164753478,-1.248946378924));
#11910=CARTESIAN_POINT('Ctrl Pts',(-1.291790116112,3.250581420145,-2.795689854368));
#11911=CARTESIAN_POINT('Ctrl Pts',(0.8733960180478,3.112998086811,-2.953266681808));
#11912=CARTESIAN_POINT('Ctrl Pts',(2.604594646812,2.975414753478,-1.643376524728));
#11913=CARTESIAN_POINT('Ctrl Pts',(3.041583038692,2.837831420145,0.4830976119985));
#11914=CARTESIAN_POINT('Ctrl Pts',(1.967213008604,2.700248086811,2.369534101977));
#11915=CARTESIAN_POINT('Ctrl Pts',(-0.08462640871746,2.562664753478,3.078515543247));
#11916=CARTESIAN_POINT('Ctrl Pts',(-2.094529967139,2.425081420145,2.257956523383));
#11917=CARTESIAN_POINT('Ctrl Pts',(-3.063242229715,2.287498086811,0.3148260017099));
#11918=CARTESIAN_POINT('Ctrl Pts',(-2.695373355482,2.195775864589,-1.083386736722));
#11919=CARTESIAN_POINT('Ctrl Pts',(-2.302458293298,2.149914753478,-1.63627193969));
#11920=CARTESIAN_POINT('',(-2.80462878822583,2.1166580354494,-0.49452709968698));
#11921=CARTESIAN_POINT('Ctrl Pts',(2.8478481444634,6.34999057338997,3.43324101593387E-6));
#11922=CARTESIAN_POINT('Ctrl Pts',(2.84809696575054,6.34115918425508,0.13170913080596));
#11923=CARTESIAN_POINT('Ctrl Pts',(2.83938055714691,6.33232843183148,0.263538298043461));
#11924=CARTESIAN_POINT('Ctrl Pts',(2.82155635415381,6.32349742268422,0.394114480287347));
#11925=CARTESIAN_POINT('Ctrl Pts',(2.80378836361778,6.31469426402333,0.524278862461372));
#11926=CARTESIAN_POINT('Ctrl Pts',(2.77696985655664,6.30589085025552,0.653196924687804));
#11927=CARTESIAN_POINT('Ctrl Pts',(2.7410111732741,6.29708629637187,0.77950469363509));
#11928=CARTESIAN_POINT('Ctrl Pts',(2.71536342294656,6.29080639457517,0.869594480764798));
#11929=CARTESIAN_POINT('Ctrl Pts',(2.68506694171866,6.28452591276246,0.958356302134713));
#11930=CARTESIAN_POINT('Ctrl Pts',(2.65041891146736,6.27824452980137,1.04538327500442));
#11931=CARTESIAN_POINT('Ctrl Pts',(2.5997071381679,6.26905093159623,1.17275825381554));
#11932=CARTESIAN_POINT('Ctrl Pts',(2.53970189234722,6.25985740260528,1.29636375830609));
#11933=CARTESIAN_POINT('Ctrl Pts',(2.4712791398385,6.25066444347172,1.41511872849825));
#11934=CARTESIAN_POINT('Ctrl Pts',(2.40117573256152,6.24124567947012,1.53679065393686));
#11935=CARTESIAN_POINT('Ctrl Pts',(2.32223565051641,6.2318275136643,1.65337194442108));
#11936=CARTESIAN_POINT('Ctrl Pts',(2.23534963126661,6.22241048450276,1.7636827323246));
#11937=CARTESIAN_POINT('Ctrl Pts',(2.18637417655564,6.21710234299513,1.82586213752406));
#11938=CARTESIAN_POINT('Ctrl Pts',(2.1348731925072,6.21179456263259,1.88604881870501));
#11939=CARTESIAN_POINT('Ctrl Pts',(2.08100037887293,6.20648723984907,1.94402707460256));
#11940=CARTESIAN_POINT('Ctrl Pts',(1.9944833156645,6.19796394303658,2.03713727419703));
#11941=CARTESIAN_POINT('Ctrl Pts',(1.90176153167035,6.18944086409824,2.1246380745346));
#11942=CARTESIAN_POINT('Ctrl Pts',(1.80356554015024,6.18091740126049,2.20548528729524));
#11943=CARTESIAN_POINT('Ctrl Pts',(1.72132980638225,6.17377929704813,2.27319202116031));
#11944=CARTESIAN_POINT('Ctrl Pts',(1.6352558172579,6.16664092358867,2.33623234091894));
#11945=CARTESIAN_POINT('Ctrl Pts',(1.54579372034786,6.15950192742754,2.39401161664401));
#11946=CARTESIAN_POINT('Ctrl Pts',(1.44237556169335,6.15124924989005,2.46080444299466));
#11947=CARTESIAN_POINT('Ctrl Pts',(1.33442994880244,6.14299574021431,2.52056554350765));
#11948=CARTESIAN_POINT('Ctrl Pts',(1.22308284077281,6.13474085238257,2.57304695358816));
#11949=CARTESIAN_POINT('Ctrl Pts',(1.09978565476745,6.1256000272776,2.63116081298718));
#11950=CARTESIAN_POINT('Ctrl Pts',(0.972339627953733,6.11645960925327,2.68034830888395));
#11951=CARTESIAN_POINT('Ctrl Pts',(0.842080652999161,6.1073198587453,2.72037778091316));
#11952=CARTESIAN_POINT('Ctrl Pts',(0.709835318182901,6.09804073332239,2.76101767488489));
#11953=CARTESIAN_POINT('Ctrl Pts',(0.574689381761339,6.0887622959294,2.79221849312912));
#11954=CARTESIAN_POINT('Ctrl Pts',(0.438018273662977,6.07948481909915,2.8136898385709));
#11955=CARTESIAN_POINT('Ctrl Pts',(0.356995911669598,6.0739848776954,2.82641863800097));
#11956=CARTESIAN_POINT('Ctrl Pts',(0.275437198421243,6.06848527387585,2.83572713385917));
#11957=CARTESIAN_POINT('Ctrl Pts',(0.19362774091322,6.0629860644215,2.84154620372221));
#11958=CARTESIAN_POINT('Ctrl Pts',(0.0703208226356168,6.05469740695531,
2.85031696927805));
#11959=CARTESIAN_POINT('Ctrl Pts',(-0.0536460153404707,6.046408497496,2.85116138367029));
#11960=CARTESIAN_POINT('Ctrl Pts',(-0.177122198901636,6.03811907683254,
2.8438099188984));
#11961=CARTESIAN_POINT('Ctrl Pts',(-0.257570601659661,6.03271827294525,
2.83902022114639));
#11962=CARTESIAN_POINT('Ctrl Pts',(-0.337810365944785,6.02731725205642,
2.8307524461649));
#11963=CARTESIAN_POINT('Ctrl Pts',(-0.417522325443764,6.0219159424764,2.81894395536511));
#11964=CARTESIAN_POINT('Ctrl Pts',(-0.539700032319504,6.01363713936129,
2.80084460946207));
#11965=CARTESIAN_POINT('Ctrl Pts',(-0.66063668500771,6.00535765802631,2.77442476750783));
#11966=CARTESIAN_POINT('Ctrl Pts',(-0.779302709057901,5.99707724032767,
2.74024834526268));
#11967=CARTESIAN_POINT('Ctrl Pts',(-0.80720319833987,5.99513036710005,2.73221286155807));
#11968=CARTESIAN_POINT('Ctrl Pts',(-0.834978242685584,5.99318344210992,
2.72374880563183));
#11969=CARTESIAN_POINT('Ctrl Pts',(-0.862614625334214,5.99123646200206,
2.71486388828898));
#11970=CARTESIAN_POINT('Ctrl Pts',(-0.991268977026622,5.98217277712265,
2.67350235066958));
#11971=CARTESIAN_POINT('Ctrl Pts',(-1.11695009844818,5.97310986356814,2.62301486270993));
#11972=CARTESIAN_POINT('Ctrl Pts',(-1.23853382309703,5.96404772924091,2.56407752716352));
#11973=CARTESIAN_POINT('Ctrl Pts',(-1.36087184752588,5.95492937385326,2.50477454712509));
#11974=CARTESIAN_POINT('Ctrl Pts',(-1.47906260614583,5.9458118073915,2.43691597684037));
#11975=CARTESIAN_POINT('Ctrl Pts',(-1.59194254846901,5.93669503790605,2.361142032262));
#11976=CARTESIAN_POINT('Ctrl Pts',(-1.66297811258364,5.93095783739041,2.31345734366688));
#11977=CARTESIAN_POINT('Ctrl Pts',(-1.73191005931691,5.92522095249404,2.26263706352174));
#11978=CARTESIAN_POINT('Ctrl Pts',(-1.79844164777402,5.91948438522322,2.20883254135779));
#11979=CARTESIAN_POINT('Ctrl Pts',(-1.89364470256363,5.91127567202618,2.13184122053871));
#11980=CARTESIAN_POINT('Ctrl Pts',(-1.98397218151525,5.90306626998173,2.04870013519556));
#11981=CARTESIAN_POINT('Ctrl Pts',(-2.068411895023,5.89485622416037,1.95995768846063));
#11982=CARTESIAN_POINT('Ctrl Pts',(-2.10449982580334,5.8913474064134,1.92203085117033));
#11983=CARTESIAN_POINT('Ctrl Pts',(-2.13951267118782,5.88783847107766,1.88308144487671));
#11984=CARTESIAN_POINT('Ctrl Pts',(-2.17337325061447,5.88432942167148,1.84315455464047));
#11985=CARTESIAN_POINT('Ctrl Pts',(-2.25261903776763,5.87611699923038,1.74971144471963));
#11986=CARTESIAN_POINT('Ctrl Pts',(-2.32555045296493,5.86790395199546,1.65091252666336));
#11987=CARTESIAN_POINT('Ctrl Pts',(-2.39177095388154,5.85969032506734,1.54783633976085));
#11988=CARTESIAN_POINT('Ctrl Pts',(-2.4239061599349,5.85570445075158,1.4978159614874));
#11989=CARTESIAN_POINT('Ctrl Pts',(-2.45446166492524,5.85171843992237,1.44678875290166));
#11990=CARTESIAN_POINT('Ctrl Pts',(-2.48339614733578,5.84773229773376,1.39487982678156));
#11991=CARTESIAN_POINT('Ctrl Pts',(-2.54955855534775,5.83861747196516,1.27618340426768));
#11992=CARTESIAN_POINT('Ctrl Pts',(-2.60728825313002,5.82950370458883,1.15281098055722));
#11993=CARTESIAN_POINT('Ctrl Pts',(-2.65617001320165,5.8203907802979,1.026027535649));
#11994=CARTESIAN_POINT('Ctrl Pts',(-2.70494098821188,5.81129850943425,0.899531431288816));
#11995=CARTESIAN_POINT('Ctrl Pts',(-2.74490449140401,5.80220707783884,0.769638550200807));
#11996=CARTESIAN_POINT('Ctrl Pts',(-2.77560145945706,5.79311627166539,0.637585044842814));
#11997=CARTESIAN_POINT('Ctrl Pts',(-2.79488703263908,5.78740491256833,0.554621556816175));
#11998=CARTESIAN_POINT('Ctrl Pts',(-2.81051409637919,5.7816938003293,0.47080491634668));
#11999=CARTESIAN_POINT('Ctrl Pts',(-2.82235825676456,5.77598288191934,0.386440773001788));
#12000=CARTESIAN_POINT('Ctrl Pts',(-2.83958163538217,5.76767825695407,0.263761280720222));
#12001=CARTESIAN_POINT('Ctrl Pts',(-2.84880240909353,5.75937251212854,0.139905880303724));
#12002=CARTESIAN_POINT('Ctrl Pts',(-2.84961906389546,5.7510660046385,0.0159905663491347));
#12003=CARTESIAN_POINT('Ctrl Pts',(-2.84976071832129,5.74962518344168,-0.00550340222553886));
#12004=CARTESIAN_POINT('Ctrl Pts',(-2.84964964004326,5.74818433929835,-0.026999149914304));
#12005=CARTESIAN_POINT('Ctrl Pts',(-2.84928389354478,5.74674347407265,-0.0484908313339417));
#12006=CARTESIAN_POINT('Ctrl Pts',(-2.84717139437973,5.73842124378764,-0.1726236917816));
#12007=CARTESIAN_POINT('Ctrl Pts',(-2.83655873600505,5.730098310184,-0.296620339600148));
#12008=CARTESIAN_POINT('Ctrl Pts',(-2.81787179531194,5.72177503245665,-0.419370041283346));
#12009=CARTESIAN_POINT('Ctrl Pts',(-2.8047403931637,5.71592622559071,-0.505626840769667));
#12010=CARTESIAN_POINT('Ctrl Pts',(-2.78762313245978,5.71007724879857,-0.591267886240161));
#12011=CARTESIAN_POINT('Ctrl Pts',(-2.76668249612696,5.70422822671777,-0.675912222910682));
#12012=CARTESIAN_POINT('Ctrl Pts',(-2.73335868244143,5.69492040440685,-0.810610713439508));
#12013=CARTESIAN_POINT('Ctrl Pts',(-2.69033017548373,5.68561390947412,-0.942904815438035));
#12014=CARTESIAN_POINT('Ctrl Pts',(-2.63814095147965,5.67630828772023,-1.07148137412761));
#12015=CARTESIAN_POINT('Ctrl Pts',(-2.58654876642552,5.6671091212499,-1.19858703120764));
#12016=CARTESIAN_POINT('Ctrl Pts',(-2.52600370630068,5.65791080809458,-1.32206085512863));
#12017=CARTESIAN_POINT('Ctrl Pts',(-2.45698549554103,5.64871290946517,-1.44061470392629));
#12018=CARTESIAN_POINT('Ctrl Pts',(-2.41638579800083,5.64330228090425,-1.51035355039066));
#12019=CARTESIAN_POINT('Ctrl Pts',(-2.37285328242831,5.6378917957832,-1.57838946707628));
#12020=CARTESIAN_POINT('Ctrl Pts',(-2.32647920766074,5.63248136478523,-1.64445463159885));
#12021=CARTESIAN_POINT('Ctrl Pts',(-2.25985477999425,5.62470833922137,-1.73936873602186));
#12022=CARTESIAN_POINT('Ctrl Pts',(-2.18737469347683,5.61693403277976,-1.83019474974451));
#12023=CARTESIAN_POINT('Ctrl Pts',(-2.10939700128704,5.60915897176398,-1.91604133255032));
#12024=CARTESIAN_POINT('Ctrl Pts',(-2.02300955965761,5.60054538484182,-2.01114631005047));
#12025=CARTESIAN_POINT('Ctrl Pts',(-1.92987476389789,5.59193087181,-2.1001385814422));
#12026=CARTESIAN_POINT('Ctrl Pts',(-1.8311472911516,5.58331614827954,-2.18241178621735));
#12027=CARTESIAN_POINT('Ctrl Pts',(-1.74484421292693,5.57578554774807,-2.25433128977591));
#12028=CARTESIAN_POINT('Ctrl Pts',(-1.654268601442,5.56825478636485,-2.32111677068052));
#12029=CARTESIAN_POINT('Ctrl Pts',(-1.56020840510456,5.5607243421452,-2.38239123466756));
#12030=CARTESIAN_POINT('Ctrl Pts',(-1.43943537989252,5.55105527313395,-2.46106747256751));
#12031=CARTESIAN_POINT('Ctrl Pts',(-1.31278466650881,5.54138780920491,-2.5307545227796));
#12032=CARTESIAN_POINT('Ctrl Pts',(-1.18168851433157,5.5317212023782,-2.59072682747743));
#12033=CARTESIAN_POINT('Ctrl Pts',(-1.05343463133871,5.52226417530075,-2.64939888475589));
#12034=CARTESIAN_POINT('Ctrl Pts',(-0.920924786554568,5.51280796856319,
-2.6987732923217));
#12035=CARTESIAN_POINT('Ctrl Pts',(-0.785483990431386,5.50335188178882,
-2.73812465054624));
#12036=CARTESIAN_POINT('Ctrl Pts',(-0.716865969063655,5.49856116892452,
-2.75806112771405));
#12037=CARTESIAN_POINT('Ctrl Pts',(-0.647495507787036,5.49377048685132,
-2.77542419804366));
#12038=CARTESIAN_POINT('Ctrl Pts',(-0.577544734694411,5.48897974449455,
-2.79011435409674));
#12039=CARTESIAN_POINT('Ctrl Pts',(-0.492851432512891,5.48317932554051,
-2.80790054530938));
#12040=CARTESIAN_POINT('Ctrl Pts',(-0.407339492713478,5.47737808128343,
-2.82176053702046));
#12041=CARTESIAN_POINT('Ctrl Pts',(-0.321359348342017,5.47157630891338,
-2.83151871774004));
#12042=CARTESIAN_POINT('Ctrl Pts',(-0.185517346254951,5.46240995567958,
-2.84693589126732));
#12043=CARTESIAN_POINT('Ctrl Pts',(-0.0485070604358834,5.45324228419315,
-2.85211158994836));
#12044=CARTESIAN_POINT('Ctrl Pts',(0.0881700098645867,5.44407446649292,
-2.84741519824236));
#12045=CARTESIAN_POINT('Ctrl Pts',(0.22162178721207,5.43512299011284,-2.84282963155654));
#12046=CARTESIAN_POINT('Ctrl Pts',(0.354754767946376,5.42617137433824,-2.82883289177504));
#12047=CARTESIAN_POINT('Ctrl Pts',(0.486182151957727,5.41722071017753,-2.80581552730152));
#12048=CARTESIAN_POINT('Ctrl Pts',(0.637663211695356,5.40690432061671,-2.77928608833381));
#12049=CARTESIAN_POINT('Ctrl Pts',(0.787088749257628,5.39658988396729,-2.74074587821702));
#12050=CARTESIAN_POINT('Ctrl Pts',(0.932540277416806,5.38627621170946,-2.69066540502931));
#12051=CARTESIAN_POINT('Ctrl Pts',(1.07298509277952,5.37631755528078,-2.64230879510475));
#12052=CARTESIAN_POINT('Ctrl Pts',(1.2097258874806,5.36635961152581,-2.58319216877987));
#12053=CARTESIAN_POINT('Ctrl Pts',(1.34101116849616,5.35640131048165,-2.51369800567432));
#12054=CARTESIAN_POINT('Ctrl Pts',(1.38901313964186,5.35276024671819,-2.48828878396734));
#12055=CARTESIAN_POINT('Ctrl Pts',(1.43628546270362,5.34911913519016,-2.46149186313972));
#12056=CARTESIAN_POINT('Ctrl Pts',(1.48274123461023,5.34547792359802,-2.43332471124822));
#12057=CARTESIAN_POINT('Ctrl Pts',(1.53157103395927,5.34165063531641,-2.40371813452701));
#12058=CARTESIAN_POINT('Ctrl Pts',(1.57947953162742,5.33782297139469,-2.37260912009654));
#12059=CARTESIAN_POINT('Ctrl Pts',(1.62636044473214,5.33399503167055,-2.34002601055496));
#12060=CARTESIAN_POINT('Ctrl Pts',(1.75117389214106,5.32380371239363,-2.25327833522488));
#12061=CARTESIAN_POINT('Ctrl Pts',(1.86870088347843,5.31361043819798,-2.15607963389188));
#12062=CARTESIAN_POINT('Ctrl Pts',(1.97776383319767,5.30341709312524,-2.05014842743312));
#12063=CARTESIAN_POINT('Ctrl Pts',(2.08369263963999,5.29351667433051,-1.94726136730815));
#12064=CARTESIAN_POINT('Ctrl Pts',(2.18163634605226,5.28361618867375,-1.83613768070385));
#12065=CARTESIAN_POINT('Ctrl Pts',(2.27055708134304,5.27371736239433,-1.71837496386946));
#12066=CARTESIAN_POINT('Ctrl Pts',(2.37798703845376,5.2617580541501,-1.57609944649558));
#12067=CARTESIAN_POINT('Ctrl Pts',(2.47243782432304,5.24980145815805,-1.42389682933471));
#12068=CARTESIAN_POINT('Ctrl Pts',(2.55208901765524,5.23784528967073,-1.26431845019061));
#12069=CARTESIAN_POINT('Ctrl Pts',(2.62502815371991,5.2268966451668,-1.11818744295228));
#12070=CARTESIAN_POINT('Ctrl Pts',(2.68555690314024,5.21594835915329,-0.965870248777373));
#12071=CARTESIAN_POINT('Ctrl Pts',(2.73222929239438,5.20499867717148,-0.809323905587983));
#12072=CARTESIAN_POINT('Ctrl Pts',(2.73652421232884,5.20399105771656,-0.794918086199347));
#12073=CARTESIAN_POINT('Ctrl Pts',(2.74070175754344,5.20298342644034,-0.780476458486443));
#12074=CARTESIAN_POINT('Ctrl Pts',(2.74476077843502,5.20197578197562,-0.76600055127141));
#12075=CARTESIAN_POINT('Ctrl Pts',(2.75222850003782,5.20012193383388,-0.739368009109834));
#12076=CARTESIAN_POINT('Ctrl Pts',(2.75929326713199,5.1982680033424,-0.712625755318726));
#12077=CARTESIAN_POINT('Ctrl Pts',(2.76594836371704,5.19641400225846,-0.685783942329835));
#12078=CARTESIAN_POINT('Ctrl Pts',(2.81024179225335,5.18407457735774,-0.50713650871018));
#12079=CARTESIAN_POINT('Ctrl Pts',(2.83638460267271,5.17173202545407,-0.324080379512753));
#12080=CARTESIAN_POINT('Ctrl Pts',(2.84485026731554,5.15938981280454,-0.140202555747719));
#12081=CARTESIAN_POINT('Ctrl Pts',(2.85152140085033,5.14966387253007,0.00469729183389342));
#12082=CARTESIAN_POINT('Ctrl Pts',(2.84721632851365,5.1399381429254,0.150107288936105));
#12083=CARTESIAN_POINT('Ctrl Pts',(2.83218569049158,5.1302143201883,0.294285196709865));
#12084=CARTESIAN_POINT('Ctrl Pts',(2.81110865098778,5.11657887798971,0.49646180779319));
#12085=CARTESIAN_POINT('Ctrl Pts',(2.76890298599158,5.1029469832523,0.696619041135436));
#12086=CARTESIAN_POINT('Ctrl Pts',(2.70601952727829,5.08931459937678,0.890024566844041));
#12087=CARTESIAN_POINT('Ctrl Pts',(2.65915327878379,5.07915455564898,1.03416726531414));
#12088=CARTESIAN_POINT('Ctrl Pts',(2.60080132238486,5.06899424022782,1.17455881312527));
#12089=CARTESIAN_POINT('Ctrl Pts',(2.53114783776104,5.05883198207297,1.30922135465441));
#12090=CARTESIAN_POINT('Ctrl Pts',(2.53032809415689,5.05871238366133,1.31080618214344));
#12091=CARTESIAN_POINT('Ctrl Pts',(2.52950678519412,5.05859278498061,1.31239021592857));
#12092=CARTESIAN_POINT('Ctrl Pts',(2.52868391319439,5.05847318602808,1.31397345381782));
#12093=CARTESIAN_POINT('Ctrl Pts',(2.43719290793056,5.04517557911134,1.49000572385092));
#12094=CARTESIAN_POINT('Ctrl Pts',(2.32655093361843,5.0318746244084,1.65587647992433));
#12095=CARTESIAN_POINT('Ctrl Pts',(2.20012636487033,5.01857424917523,1.80870322130724));
#12096=CARTESIAN_POINT('Ctrl Pts',(2.09916138403714,5.00795232541635,1.93075346175748));
#12097=CARTESIAN_POINT('Ctrl Pts',(1.98812917464779,4.99733077123822,2.04448488234765));
#12098=CARTESIAN_POINT('Ctrl Pts',(1.86872280618781,4.98671158699582,2.14843627152901));
#12099=CARTESIAN_POINT('Ctrl Pts',(1.73420524933564,4.97474851719918,2.26554298103214));
#12100=CARTESIAN_POINT('Ctrl Pts',(1.58882199632064,4.96278798301116,2.37043814307767));
#12101=CARTESIAN_POINT('Ctrl Pts',(1.4349635770105,4.95082703617151,2.4608589775063));
#12102=CARTESIAN_POINT('Ctrl Pts',(1.30815421469591,4.94096888184876,2.53538339030905));
#12103=CARTESIAN_POINT('Ctrl Pts',(1.17558913257157,4.93111044721276,2.60007530364507));
#12104=CARTESIAN_POINT('Ctrl Pts',(1.03863029203751,4.92125008160984,2.65367989990671));
#12105=CARTESIAN_POINT('Ctrl Pts',(1.00955535153907,4.91915682832236,2.66505959938922));
#12106=CARTESIAN_POINT('Ctrl Pts',(0.980282458753524,4.91706348801221,2.67593968041636));
#12107=CARTESIAN_POINT('Ctrl Pts',(0.95082918475627,4.91497004488722,2.68631959875166));
#12108=CARTESIAN_POINT('Ctrl Pts',(0.799276180692962,4.90419814922434,2.73972988535656));
#12109=CARTESIAN_POINT('Ctrl Pts',(0.643155172613163,4.89342481534808,2.77982888277722));
#12110=CARTESIAN_POINT('Ctrl Pts',(0.484778766588518,4.88265174521157,2.80666919304322));
#12111=CARTESIAN_POINT('Ctrl Pts',(0.318147226613579,4.87131714486192,2.8349085144503));
#12112=CARTESIAN_POINT('Ctrl Pts',(0.149017878869776,4.8599828364626,2.84847134663192));
#12113=CARTESIAN_POINT('Ctrl Pts',(-0.019946453562988,4.848650802215,2.84737147468315));
#12114=CARTESIAN_POINT('Ctrl Pts',(-0.0469929580676308,4.84683685775162,
2.84719541568189));
#12115=CARTESIAN_POINT('Ctrl Pts',(-0.074035272357364,4.84502297155914,
2.84664355083377));
#12116=CARTESIAN_POINT('Ctrl Pts',(-0.101062509484977,4.84320915176765,
2.84571582061425));
#12117=CARTESIAN_POINT('Ctrl Pts',(-0.250363679354825,4.83318942923648,
2.840590945791));
#12118=CARTESIAN_POINT('Ctrl Pts',(-0.399415580182845,4.82317115084706,
2.82398464559706));
#12119=CARTESIAN_POINT('Ctrl Pts',(-0.546236844382753,4.81315266285064,
2.79581809727281));
#12120=CARTESIAN_POINT('Ctrl Pts',(-0.690256359088589,4.8033253548841,2.76818904338405));
#12121=CARTESIAN_POINT('Ctrl Pts',(-0.832128210659078,4.79349784523402,
2.72943686342525));
#12122=CARTESIAN_POINT('Ctrl Pts',(-0.969978395291538,4.78366857303063,
2.67953573585256));
#12123=CARTESIAN_POINT('Ctrl Pts',(-1.02701636231628,4.77960153673822,2.65888825629657));
#12124=CARTESIAN_POINT('Ctrl Pts',(-1.08336587223442,4.77553419869001,2.6363326080126));
#12125=CARTESIAN_POINT('Ctrl Pts',(-1.13892524763199,4.77146644831613,2.61195352742645));
#12126=CARTESIAN_POINT('Ctrl Pts',(-1.27332233275196,4.76162663659521,2.55298098957416));
#12127=CARTESIAN_POINT('Ctrl Pts',(-1.40296756560452,4.75178622629293,2.4834005734629));
#12128=CARTESIAN_POINT('Ctrl Pts',(-1.52659117388361,4.74194620226236,2.40439336973659));
#12129=CARTESIAN_POINT('Ctrl Pts',(-1.65471235135068,4.73174818682945,2.32251179298352));
#12130=CARTESIAN_POINT('Ctrl Pts',(-1.77636691693109,4.72155058628551,2.23050444652182));
#12131=CARTESIAN_POINT('Ctrl Pts',(-1.89012498891916,4.71135449693192,2.12963331895248));
#12132=CARTESIAN_POINT('Ctrl Pts',(-1.93344485021052,4.70747175552471,2.09122089530429));
#12133=CARTESIAN_POINT('Ctrl Pts',(-1.97561935365505,4.70358923326113,2.05152261794535));
#12134=CARTESIAN_POINT('Ctrl Pts',(-2.01656839967359,4.69970699068146,2.01060656280138));
#12135=CARTESIAN_POINT('Ctrl Pts',(-2.11229311203592,4.6906316497299,1.91495897169792));
#12136=CARTESIAN_POINT('Ctrl Pts',(-2.2014321872198,4.68155709368734,1.81253895656524));
#12137=CARTESIAN_POINT('Ctrl Pts',(-2.2828146653471,4.67248228155625,1.70429494526024));
#12138=CARTESIAN_POINT('Ctrl Pts',(-2.36171617245722,4.66368411799132,1.59935078744963));
#12139=CARTESIAN_POINT('Ctrl Pts',(-2.43332607264819,4.65488571371377,1.48893324423344));
#12140=CARTESIAN_POINT('Ctrl Pts',(-2.49660877287086,4.64608612005862,1.37394121389828));
#12141=CARTESIAN_POINT('Ctrl Pts',(-2.54004957872659,4.64004558388936,1.2950042145735));
#12142=CARTESIAN_POINT('Ctrl Pts',(-2.57956713284195,4.63400448725897,1.21391235616628));
#12143=CARTESIAN_POINT('Ctrl Pts',(-2.6150947154906,4.62796252329951,1.13110423363072));
#12144=CARTESIAN_POINT('Ctrl Pts',(-2.67021293955555,4.61858889586747,1.00263400537312));
#12145=CARTESIAN_POINT('Ctrl Pts',(-2.7157020102016,4.60921522696859,0.870109166010463));
#12146=CARTESIAN_POINT('Ctrl Pts',(-2.75141516065125,4.59984209210928,0.735000743640519));
#12147=CARTESIAN_POINT('Ctrl Pts',(-2.78803267481489,4.59023160145956,0.596470972184675));
#12148=CARTESIAN_POINT('Ctrl Pts',(-2.81437326800116,4.58062167223881,0.455223899761565));
#12149=CARTESIAN_POINT('Ctrl Pts',(-2.83023010740115,4.57101292479062,0.312821329313767));
#12150=CARTESIAN_POINT('Ctrl Pts',(-2.83837622524724,4.56607663281642,0.239665002810554));
#12151=CARTESIAN_POINT('Ctrl Pts',(-2.84375468353297,4.56114065273264,0.166203453674323));
#12152=CARTESIAN_POINT('Ctrl Pts',(-2.84633213932709,4.5562050686467,0.0926477277248243));
#12153=CARTESIAN_POINT('Ctrl Pts',(-2.85080369569687,4.54764246109071,-0.0349620554002695));
#12154=CARTESIAN_POINT('Ctrl Pts',(-2.84684405950869,4.53908011868222,-0.162981422032098));
#12155=CARTESIAN_POINT('Ctrl Pts',(-2.834239387605,4.53051741032784,-0.290140302708813));
#12156=CARTESIAN_POINT('Ctrl Pts',(-2.82343743161624,4.52317933762787,-0.399112963254424));
#12157=CARTESIAN_POINT('Ctrl Pts',(-2.80628716758326,4.51584099617165,-0.507452912356721));
#12158=CARTESIAN_POINT('Ctrl Pts',(-2.78268445247893,4.5085019887619,-0.614359082965291));
#12159=CARTESIAN_POINT('Ctrl Pts',(-2.75691231571862,4.50048842329653,-0.731091435038663));
#12160=CARTESIAN_POINT('Ctrl Pts',(-2.72344676688929,4.4924740638305,-0.846113502585519));
#12161=CARTESIAN_POINT('Ctrl Pts',(-2.68285940366929,4.48445839326727,-0.958539835166529));
#12162=CARTESIAN_POINT('Ctrl Pts',(-2.63657534198002,4.47531767158949,-1.08674592937551));
#12163=CARTESIAN_POINT('Ctrl Pts',(-2.58104650664304,4.46617733297043,-1.21155651494625));
#12164=CARTESIAN_POINT('Ctrl Pts',(-2.51705937033925,4.45703765854587,-1.33186684914844));
#12165=CARTESIAN_POINT('Ctrl Pts',(-2.45204500968134,4.44775125937788,-1.45410859820187));
#12166=CARTESIAN_POINT('Ctrl Pts',(-2.37829801534487,4.438465545901,-1.57170557119922));
#12167=CARTESIAN_POINT('Ctrl Pts',(-2.29659335178013,4.42918081300935,-1.68348107768699));
#12168=CARTESIAN_POINT('Ctrl Pts',(-2.24825681646411,4.42368795862703,-1.74960754441592));
#12169=CARTESIAN_POINT('Ctrl Pts',(-2.19713426300355,4.41819544744109,-1.81369612736419));
#12170=CARTESIAN_POINT('Ctrl Pts',(-2.14337940984177,4.41270334051083,-1.87549783130719));
#12171=CARTESIAN_POINT('Ctrl Pts',(-2.06216813859641,4.40440602483816,-1.96886605105165));
#12172=CARTESIAN_POINT('Ctrl Pts',(-1.97488330498467,4.39610851128944,-2.05708156164466));
#12173=CARTESIAN_POINT('Ctrl Pts',(-1.88215307563072,4.38781050185156,-2.13913975278296));
#12174=CARTESIAN_POINT('Ctrl Pts',(-1.81922503464678,4.38217935565867,-2.19482559817551));
#12175=CARTESIAN_POINT('Ctrl Pts',(-1.75379029273467,4.37654798110035,-2.24767632393704));
#12176=CARTESIAN_POINT('Ctrl Pts',(-1.68605559554002,4.37091628504346,-2.297386871109));
#12177=CARTESIAN_POINT('Ctrl Pts',(-1.58640436084932,4.36263093811323,-2.37052099007613));
#12178=CARTESIAN_POINT('Ctrl Pts',(-1.48177429550487,4.35434489532274,-2.436856127471));
#12179=CARTESIAN_POINT('Ctrl Pts',(-1.37329667206734,4.34605786010788,-2.49606869218833));
#12180=CARTESIAN_POINT('Ctrl Pts',(-1.35102808158013,4.34435667429918,-2.50822401338364));
#12181=CARTESIAN_POINT('Ctrl Pts',(-1.32859742487597,4.3426554466687,-2.52007934135439));
#12182=CARTESIAN_POINT('Ctrl Pts',(-1.30601458666857,4.34095417465092,-2.53163212802679));
#12183=CARTESIAN_POINT('Ctrl Pts',(-1.1857521478759,4.33189423630173,-2.59315523186848));
#12184=CARTESIAN_POINT('Ctrl Pts',(-1.06115273222554,4.32283502699286,-2.64611431941297));
#12185=CARTESIAN_POINT('Ctrl Pts',(-0.933490708804636,4.31377658423978,
-2.69020099239149));
#12186=CARTESIAN_POINT('Ctrl Pts',(-0.804885285362792,4.30465120117936,
-2.73461345817117));
#12187=CARTESIAN_POINT('Ctrl Pts',(-0.673170621020409,4.29552659604602,
-2.77002228964768));
#12188=CARTESIAN_POINT('Ctrl Pts',(-0.539627852568289,4.28640280719315,
-2.79606489591989));
#12189=CARTESIAN_POINT('Ctrl Pts',(-0.455700474782248,4.28066879641315,
-2.81243184472943));
#12190=CARTESIAN_POINT('Ctrl Pts',(-0.371050677151256,4.27493510804125,
-2.82509843252094));
#12191=CARTESIAN_POINT('Ctrl Pts',(-0.285995403583839,4.26920175159779,
-2.83396412656041));
#12192=CARTESIAN_POINT('Ctrl Pts',(-0.164183522195132,4.26099072709857,
-2.84666112729261));
#12193=CARTESIAN_POINT('Ctrl Pts',(-0.041479910489348,4.25277906620465,
-2.8515628186172));
#12194=CARTESIAN_POINT('Ctrl Pts',(0.0810094029847688,4.24456677723678,
-2.84834577334894));
#12195=CARTESIAN_POINT('Ctrl Pts',(0.13687525607919,4.2408212543333,-2.84687851899624));
#12196=CARTESIAN_POINT('Ctrl Pts',(0.192696365280209,4.23707560078048,-2.84372312835945));
#12197=CARTESIAN_POINT('Ctrl Pts',(0.248367412713555,4.2333298173677,-2.83885251761691));
#12198=CARTESIAN_POINT('Ctrl Pts',(0.370431291058467,4.22511684362492,-2.82817325677034));
#12199=CARTESIAN_POINT('Ctrl Pts',(0.491772856086867,4.21690324558581,-2.80924474939128));
#12200=CARTESIAN_POINT('Ctrl Pts',(0.611351618208173,4.20868903157138,-2.78255509152167));
#12201=CARTESIAN_POINT('Ctrl Pts',(0.665887443384615,4.20494280664393,-2.77038284212073));
#12202=CARTESIAN_POINT('Ctrl Pts',(0.720056775219937,4.20119645359587,-2.75659701156376));
#12203=CARTESIAN_POINT('Ctrl Pts',(0.773762155636671,4.19744997321655,-2.74124726262043));
#12204=CARTESIAN_POINT('Ctrl Pts',(0.904265963911871,4.1883460444605,-2.70394744875398));
#12205=CARTESIAN_POINT('Ctrl Pts',(1.03210179914571,4.17924314089706,-2.65739809823362));
#12206=CARTESIAN_POINT('Ctrl Pts',(1.15608961781954,4.17014107439263,-2.60220541100469));
#12207=CARTESIAN_POINT('Ctrl Pts',(1.27992336361626,4.16105031852814,-2.5470813087078));
#12208=CARTESIAN_POINT('Ctrl Pts',(1.39991978605433,4.15196039764364,-2.48333477778042));
#12209=CARTESIAN_POINT('Ctrl Pts',(1.51488473647243,4.14287112430601,-2.41152225575072));
#12210=CARTESIAN_POINT('Ctrl Pts',(1.58728265227502,4.13714725417506,-2.36629910813426));
#12211=CARTESIAN_POINT('Ctrl Pts',(1.65768480452553,4.13142364084257,-2.31787630256474));
#12212=CARTESIAN_POINT('Ctrl Pts',(1.72578611389249,4.12570023749965,-2.2663846186789));
#12213=CARTESIAN_POINT('Ctrl Pts',(1.82435957315917,4.11741587892366,-2.19185281523377));
#12214=CARTESIAN_POINT('Ctrl Pts',(1.91812685833765,4.10913045284344,-2.11087324313886));
#12215=CARTESIAN_POINT('Ctrl Pts',(2.00602383790393,4.10084427739672,-2.02395239693411));
#12216=CARTESIAN_POINT('Ctrl Pts',(2.02405849606512,4.09914412407652,-2.00611802132622));
#12217=CARTESIAN_POINT('Ctrl Pts',(2.04184612028,4.09744393920902,-1.98803367128797));
#12218=CARTESIAN_POINT('Ctrl Pts',(2.05937768551325,4.09574372554221,-1.96970393933037));
#12219=CARTESIAN_POINT('Ctrl Pts',(2.14496407303129,4.0874435456202,-1.88022102542318));
#12220=CARTESIAN_POINT('Ctrl Pts',(2.22444454601499,4.07914267934137,-1.78488749043672));
#12221=CARTESIAN_POINT('Ctrl Pts',(2.29734399251735,4.07084144642509,-1.68478489258555));
#12222=CARTESIAN_POINT('Ctrl Pts',(2.34680041128402,4.06520972669216,-1.61687332073572));
#12223=CARTESIAN_POINT('Ctrl Pts',(2.39322871986781,4.05957783821317,-1.54676757298662));
#12224=CARTESIAN_POINT('Ctrl Pts',(2.43649261093021,4.05394588081884,-1.47481174068824));
#12225=CARTESIAN_POINT('Ctrl Pts',(2.50775104962519,4.04466968117841,-1.3562958111528));
#12226=CARTESIAN_POINT('Ctrl Pts',(2.57049079385341,4.03539477674111,-1.23266463282099));
#12227=CARTESIAN_POINT('Ctrl Pts',(2.62418232290552,4.02612074408822,-1.10522080479152));
#12228=CARTESIAN_POINT('Ctrl Pts',(2.67732164753879,4.01694209262305,-0.979087705777112));
#12229=CARTESIAN_POINT('Ctrl Pts',(2.72159833392014,4.00776429510233,-0.849218780956081));
#12230=CARTESIAN_POINT('Ctrl Pts',(2.75645283976302,3.99858694103764,-0.71685792494221));
#12231=CARTESIAN_POINT('Ctrl Pts',(2.77720016500195,3.99312407346834,-0.63806943943041));
#12232=CARTESIAN_POINT('Ctrl Pts',(2.79460803017755,3.98766136302824,-0.558397714916988));
#12233=CARTESIAN_POINT('Ctrl Pts',(2.80854958934038,3.98219872313878,-0.478104491334957));
#12234=CARTESIAN_POINT('Ctrl Pts',(2.8289977693348,3.97418663192289,-0.360337872195623));
#12235=CARTESIAN_POINT('Ctrl Pts',(2.84198145600201,3.96617321355946,-0.24125180620398));
#12236=CARTESIAN_POINT('Ctrl Pts',(2.84709160218678,3.95815901551443,-0.121817505725509));
#12237=CARTESIAN_POINT('Ctrl Pts',(2.85255389365086,3.94959255107487,0.00584713172955927));
#12238=CARTESIAN_POINT('Ctrl Pts',(2.84901944856095,3.94102519579393,0.13390865241372));
#12239=CARTESIAN_POINT('Ctrl Pts',(2.83687638457245,3.93245761829523,0.261142010808346));
#12240=CARTESIAN_POINT('Ctrl Pts',(2.82647528994478,3.92511909283096,0.37012325324529));
#12241=CARTESIAN_POINT('Ctrl Pts',(2.80975935061011,3.91778040433192,0.478496429154096));
#12242=CARTESIAN_POINT('Ctrl Pts',(2.7870018996455,3.91044197297679,0.585499256888617));
#12243=CARTESIAN_POINT('Ctrl Pts',(2.75718958450986,3.90082861036861,0.725673216871521));
#12244=CARTESIAN_POINT('Ctrl Pts',(2.71698441767795,3.8912168171005,0.863652500268121));
#12245=CARTESIAN_POINT('Ctrl Pts',(2.6668868192048,3.88160588597332,0.997942599994107));
#12246=CARTESIAN_POINT('Ctrl Pts',(2.6178084021306,3.87219047883392,1.12950071304055));
#12247=CARTESIAN_POINT('Ctrl Pts',(2.55923541270253,3.86277589911363,1.25751936135917));
#12248=CARTESIAN_POINT('Ctrl Pts',(2.49159411524659,3.8533614819027,1.3805726182506));
#12249=CARTESIAN_POINT('Ctrl Pts',(2.45647354948705,3.8484733488955,1.4444640597682));
#12250=CARTESIAN_POINT('Ctrl Pts',(2.41890760236793,3.84358525969874,1.50701644777642));
#12251=CARTESIAN_POINT('Ctrl Pts',(2.37895180791164,3.83869712124206,1.56802637965971));
#12252=CARTESIAN_POINT('Ctrl Pts',(2.32958431699072,3.83265756842715,1.64340736755695));
#12253=CARTESIAN_POINT('Ctrl Pts',(2.27658552809973,3.82661713171428,1.71640518801221));
#12254=CARTESIAN_POINT('Ctrl Pts',(2.22009732330164,3.82057613731894,1.78659955199873));
#12255=CARTESIAN_POINT('Ctrl Pts',(2.13518671489279,3.81149557773424,1.89211266175804));
#12256=CARTESIAN_POINT('Ctrl Pts',(2.04239038531967,3.80241375807755,1.99128929097583));
#12257=CARTESIAN_POINT('Ctrl Pts',(1.94300077141682,3.79333178629112,2.08335525699706));
#12258=CARTESIAN_POINT('Ctrl Pts',(1.84671862500594,3.78453376703233,2.17254273315104));
#12259=CARTESIAN_POINT('Ctrl Pts',(1.74425017248423,3.77573560500794,2.25505686398576));
#12260=CARTESIAN_POINT('Ctrl Pts',(1.63679510037212,3.76693830745429,2.33023339542586));
#12261=CARTESIAN_POINT('Ctrl Pts',(1.51201676441845,3.7567227622217,2.41752943749707));
#12262=CARTESIAN_POINT('Ctrl Pts',(1.38035145290207,3.74650912030626,2.49505664498431));
#12263=CARTESIAN_POINT('Ctrl Pts',(1.24344279684043,3.73629626040805,2.56183339412736));
#12264=CARTESIAN_POINT('Ctrl Pts',(1.11100607355229,3.72641698951877,2.62642897268857));
#12265=CARTESIAN_POINT('Ctrl Pts',(0.973661763850657,3.716538450394,2.68096532304448));
#12266=CARTESIAN_POINT('Ctrl Pts',(0.832885022088923,3.70665962806103,2.72450770689853));
#12267=CARTESIAN_POINT('Ctrl Pts',(0.778429129104624,3.7028382575346,2.74135096783613));
#12268=CARTESIAN_POINT('Ctrl Pts',(0.723459584799259,3.69901684463083,2.75654863331248));
#12269=CARTESIAN_POINT('Ctrl Pts',(0.66806180137864,3.69519533060128,2.77004446035488));
#12270=CARTESIAN_POINT('Ctrl Pts',(0.609112947181974,3.6911288524964,2.78440538766031));
#12271=CARTESIAN_POINT('Ctrl Pts',(0.54970265226331,3.68706195029126,2.79683335328153));
#12272=CARTESIAN_POINT('Ctrl Pts',(0.489945752046593,3.68299474226145,2.8072625801369));
#12273=CARTESIAN_POINT('Ctrl Pts',(0.342616168957259,3.67296711262878,2.83297565492781));
#12274=CARTESIAN_POINT('Ctrl Pts',(0.193179931634859,3.66293762400927,2.84653552760749));
#12275=CARTESIAN_POINT('Ctrl Pts',(0.0435912834424511,3.65290804896259,
2.84831532521404));
#12276=CARTESIAN_POINT('Ctrl Pts',(-0.102943903755338,3.64308320145753,
2.85005879290761));
#12277=CARTESIAN_POINT('Ctrl Pts',(-0.249624082421185,3.63325827101767,
2.84049861746464));
#12278=CARTESIAN_POINT('Ctrl Pts',(-0.394624710814754,3.62343492385677,
2.82003242443467));
#12279=CARTESIAN_POINT('Ctrl Pts',(-0.571154976497794,3.61147554062221,
2.7951159634984));
#12280=CARTESIAN_POINT('Ctrl Pts',(-0.745496729775374,3.59951886296536,
2.75400322734476));
#12281=CARTESIAN_POINT('Ctrl Pts',(-0.914569285802567,3.58756265879809,
2.69722852032646));
#12282=CARTESIAN_POINT('Ctrl Pts',(-1.06695640580188,3.57678638876359,2.64605679680953));
#12283=CARTESIAN_POINT('Ctrl Pts',(-1.21506381218767,3.56601050337461,2.58216093989508));
#12284=CARTESIAN_POINT('Ctrl Pts',(-1.35660426622524,3.55523336831249,2.5058952187549));
#12285=CARTESIAN_POINT('Ctrl Pts',(-1.37210206020685,3.55405333946462,2.49754459954765));
#12286=CARTESIAN_POINT('Ctrl Pts',(-1.38752108339747,3.55287329563457,2.48904564691914));
#12287=CARTESIAN_POINT('Ctrl Pts',(-1.40285830175433,3.55169323467695,2.48039880218197));
#12288=CARTESIAN_POINT('Ctrl Pts',(-1.4300617271585,3.54960017585195,2.46506200574888));
#12289=CARTESIAN_POINT('Ctrl Pts',(-1.45700064554427,3.54750701042459,2.44926397377593));
#12290=CARTESIAN_POINT('Ctrl Pts',(-1.48365784997017,3.5454137553533,2.43300829364778));
#12291=CARTESIAN_POINT('Ctrl Pts',(-1.63619964879767,3.53343542150859,2.33998763595633));
#12292=CARTESIAN_POINT('Ctrl Pts',(-1.779513195613,3.52145415224934,2.23197927270628));
#12293=CARTESIAN_POINT('Ctrl Pts',(-1.91158903059991,3.50947312524184,2.11162428747825));
#12294=CARTESIAN_POINT('Ctrl Pts',(-2.02014920877862,3.49962527967019,2.01269810130387));
#12295=CARTESIAN_POINT('Ctrl Pts',(-2.12111753814876,3.48977759776559,1.90543133827463));
#12296=CARTESIAN_POINT('Ctrl Pts',(-2.21340374161109,3.4799318441425,1.7912975705709));
#12297=CARTESIAN_POINT('Ctrl Pts',(-2.33818722219613,3.46661904808004,1.63697321598664));
#12298=CARTESIAN_POINT('Ctrl Pts',(-2.44734366893353,3.45330963601978,1.4697973896561));
#12299=CARTESIAN_POINT('Ctrl Pts',(-2.53808343374277,3.43999992429471,1.29318656076566));
#12300=CARTESIAN_POINT('Ctrl Pts',(-2.61036500647599,3.42939766079826,1.15250172980146));
#12301=CARTESIAN_POINT('Ctrl Pts',(-2.67095976199367,3.41879520715212,1.00583019415891));
#12302=CARTESIAN_POINT('Ctrl Pts',(-2.71843656738083,3.40819070139704,0.854910070656629));
#12303=CARTESIAN_POINT('Ctrl Pts',(-2.71897202898103,3.40807109971839,0.853207935684107));
#12304=CARTESIAN_POINT('Ctrl Pts',(-2.71950581296388,3.4079514977575,0.851505288330626));
#12305=CARTESIAN_POINT('Ctrl Pts',(-2.72003791742379,3.40783189551727,0.849802131157961));
#12306=CARTESIAN_POINT('Ctrl Pts',(-2.78064313378115,3.39420953338379,0.655817271573425));
#12307=CARTESIAN_POINT('Ctrl Pts',(-2.81946197667226,3.38058354759009,0.455223171462301));
#12308=CARTESIAN_POINT('Ctrl Pts',(-2.83688305988526,3.36695824880052,0.252781415767838));
#12309=CARTESIAN_POINT('Ctrl Pts',(-2.84989568282765,3.35678087501392,0.101568187380142));
#12310=CARTESIAN_POINT('Ctrl Pts',(-2.85096951908672,3.34660388452721,-0.0506770999019837));
#12311=CARTESIAN_POINT('Ctrl Pts',(-2.84026065611321,3.33642907378275,-0.201987989379743));
#12312=CARTESIAN_POINT('Ctrl Pts',(-2.82729090711349,3.32410612765842,-0.385244070095902));
#12313=CARTESIAN_POINT('Ctrl Pts',(-2.79701034081176,3.31178591434536,-0.567458903452159));
#12314=CARTESIAN_POINT('Ctrl Pts',(-2.74953742834339,3.2994652189085,-0.745047684255998));
#12315=CARTESIAN_POINT('Ctrl Pts',(-2.71201735900181,3.28972759542826,-0.885404427156217));
#12316=CARTESIAN_POINT('Ctrl Pts',(-2.66375909072285,3.27998967079027,-1.02287042766145));
#12317=CARTESIAN_POINT('Ctrl Pts',(-2.60484225061453,3.27024985781717,-1.15566723149896));
#12318=CARTESIAN_POINT('Ctrl Pts',(-2.59362723400801,3.26839585200089,-1.18094554509474));
#12319=CARTESIAN_POINT('Ctrl Pts',(-2.58202606365812,3.26654177776194,-1.2060546646842));
#12320=CARTESIAN_POINT('Ctrl Pts',(-2.57004711808163,3.26468762415302,-1.23098575734892));
#12321=CARTESIAN_POINT('Ctrl Pts',(-2.49934599096278,3.25374419435236,-1.37813195986286));
#12322=CARTESIAN_POINT('Ctrl Pts',(-2.41558860934539,3.24279918690502,-1.51887089551128));
#12323=CARTESIAN_POINT('Ctrl Pts',(-2.32053943933346,3.2318544370577,-1.65153069994788));
#12324=CARTESIAN_POINT('Ctrl Pts',(-2.22030733295526,3.22031288092584,-1.79142431110442));
#12325=CARTESIAN_POINT('Ctrl Pts',(-2.10751788126752,3.20877161125327,-1.92233476579457));
#12326=CARTESIAN_POINT('Ctrl Pts',(-1.98418459168677,3.19723278017763,-2.04229092572904));
#12327=CARTESIAN_POINT('Ctrl Pts',(-1.96884192219244,3.19579734881805,-2.05721348006891));
#12328=CARTESIAN_POINT('Ctrl Pts',(-1.95333602220956,3.19436195519667,-2.07196648687955));
#12329=CARTESIAN_POINT('Ctrl Pts',(-1.93767071885483,3.19292660345666,-2.0865461270179));
#12330=CARTESIAN_POINT('Ctrl Pts',(-1.82653568299889,3.18274372582708,-2.18997909558875));
#12331=CARTESIAN_POINT('Ctrl Pts',(-1.70721454429739,3.17256239098252,-2.28483266857398));
#12332=CARTESIAN_POINT('Ctrl Pts',(-1.58112343764028,3.16238084259267,-2.36958986849931));
#12333=CARTESIAN_POINT('Ctrl Pts',(-1.45847682856542,3.15247742895588,-2.45203171107739));
#12334=CARTESIAN_POINT('Ctrl Pts',(-1.32942616321843,3.14257381328154,-2.5249204589247));
#12335=CARTESIAN_POINT('Ctrl Pts',(-1.19531110992135,3.13266837927901,-2.58689025716349));
#12336=CARTESIAN_POINT('Ctrl Pts',(-1.1434844665379,3.12884058081056,-2.61083750659531));
#12337=CARTESIAN_POINT('Ctrl Pts',(-1.09090186043034,3.12501251080862,-2.63315460308598));
#12338=CARTESIAN_POINT('Ctrl Pts',(-1.0376728971373,3.12118407600231,-2.65383209561131));
#12339=CARTESIAN_POINT('Ctrl Pts',(-0.899746226006865,3.1112638514515,-2.70741152934259));
#12340=CARTESIAN_POINT('Ctrl Pts',(-0.757621948601878,3.10134294670043,
-2.74993223899868));
#12341=CARTESIAN_POINT('Ctrl Pts',(-0.613079557174189,3.0914224103428,-2.78133826411903));
#12342=CARTESIAN_POINT('Ctrl Pts',(-0.463051255015121,3.08112535346184,
-2.81393626239366));
#12343=CARTESIAN_POINT('Ctrl Pts',(-0.310416588733038,3.0708286934687,-2.83456026641949));
#12344=CARTESIAN_POINT('Ctrl Pts',(-0.157139282858265,3.06053360293976,
-2.84309887830231));
#12345=CARTESIAN_POINT('Ctrl Pts',(-0.10200333405594,3.05683031770076,-2.84617033408585));
#12346=CARTESIAN_POINT('Ctrl Pts',(-0.0467840851091486,3.05312723554094,
-2.84767753954083));
#12347=CARTESIAN_POINT('Ctrl Pts',(0.0084273585641129,3.04942441103761,
-2.84761369930359));
#12348=CARTESIAN_POINT('Ctrl Pts',(0.145022335917836,3.04026349809047,-2.84745575639935));
#12349=CARTESIAN_POINT('Ctrl Pts',(0.281736206132755,3.03110343981126,-2.83767675257286));
#12350=CARTESIAN_POINT('Ctrl Pts',(0.417030580383158,3.02194313588785,-2.81812304454695));
#12351=CARTESIAN_POINT('Ctrl Pts',(0.549244980840984,3.0129913661047,-2.7990144763031));
#12352=CARTESIAN_POINT('Ctrl Pts',(0.680102565697361,3.00403936173425,-2.77057126889529));
#12353=CARTESIAN_POINT('Ctrl Pts',(0.808165230425777,2.99508609591237,-2.73269807790536));
#12354=CARTESIAN_POINT('Ctrl Pts',(0.891144568989746,2.98928474797492,-2.70815780815293));
#12355=CARTESIAN_POINT('Ctrl Pts',(0.972950471700694,2.98348287041621,-2.67965937474857));
#12356=CARTESIAN_POINT('Ctrl Pts',(1.05326830465212,2.977680183882,-2.64743662252163));
#12357=CARTESIAN_POINT('Ctrl Pts',(1.18358736308271,2.96826508118665,-2.59515385322933));
#12358=CARTESIAN_POINT('Ctrl Pts',(1.30991012635984,2.95884987814422,-2.53310462897821));
#12359=CARTESIAN_POINT('Ctrl Pts',(1.43108061450185,2.94943519183428,-2.46224537776815));
#12360=CARTESIAN_POINT('Ctrl Pts',(1.55546616618113,2.93977070200258,-2.38950599057501));
#12361=CARTESIAN_POINT('Ctrl Pts',(1.67442352860711,2.93010675668848,-2.30748226668282));
#12362=CARTESIAN_POINT('Ctrl Pts',(1.78668491565101,2.92044402340607,-2.21715735664828));
#12363=CARTESIAN_POINT('Ctrl Pts',(1.84292582065231,2.91560317047436,-2.17190622606571));
#12364=CARTESIAN_POINT('Ctrl Pts',(1.89748577612663,2.91076262174164,-2.12457090221474));
#12365=CARTESIAN_POINT('Ctrl Pts',(1.95020241061681,2.90592246113963,-2.07527108311025));
#12366=CARTESIAN_POINT('Ctrl Pts',(2.04397384324838,2.89731286763642,-1.98757742226459));
#12367=CARTESIAN_POINT('Ctrl Pts',(2.13200436224271,2.88870359842508,-1.89357535354423));
#12368=CARTESIAN_POINT('Ctrl Pts',(2.21323285300151,2.88009397817898,-1.79402779742342));
#12369=CARTESIAN_POINT('Ctrl Pts',(2.2842772396131,2.87256379777517,-1.70696111678932));
#12370=CARTESIAN_POINT('Ctrl Pts',(2.35011819774215,2.86503334884133,-1.61565336536314));
#12371=CARTESIAN_POINT('Ctrl Pts',(2.41006756861768,2.85750217954432,-1.52063939005921));
#12372=CARTESIAN_POINT('Ctrl Pts',(2.47195337799855,2.84972774420458,-1.42255634634576));
#12373=CARTESIAN_POINT('Ctrl Pts',(2.52756038400556,2.84195254121281,-1.32052427569478));
#12374=CARTESIAN_POINT('Ctrl Pts',(2.57669081111168,2.83417607352209,-1.21548324525062));
#12375=CARTESIAN_POINT('Ctrl Pts',(2.63456575396471,2.82501550542389,-1.09174640858425));
#12376=CARTESIAN_POINT('Ctrl Pts',(2.68344801398981,2.81585527377479,-0.963865763740706));
#12377=CARTESIAN_POINT('Ctrl Pts',(2.72311848058956,2.80669569192513,-0.833190120338741));
#12378=CARTESIAN_POINT('Ctrl Pts',(2.76346867605783,2.79737916631502,-0.700275430743322));
#12379=CARTESIAN_POINT('Ctrl Pts',(2.79428908464733,2.78806331296295,-0.564467934780335));
#12380=CARTESIAN_POINT('Ctrl Pts',(2.81530111786789,2.77874846160411,-0.427164010794746));
#12381=CARTESIAN_POINT('Ctrl Pts',(2.82757907739632,2.77330551532677,-0.346933220937656));
#12382=CARTESIAN_POINT('Ctrl Pts',(2.83650712469226,2.76786291117145,-0.266191152347382));
#12383=CARTESIAN_POINT('Ctrl Pts',(2.84202147888127,2.76242071492505,-0.185215426013762));
#12384=CARTESIAN_POINT('Ctrl Pts',(2.85045103785572,2.75410146073187,-0.0614312733763999));
#12385=CARTESIAN_POINT('Ctrl Pts',(2.85090464794611,2.74578206280165,0.0629964521132601));
#12386=CARTESIAN_POINT('Ctrl Pts',(2.84311949965228,2.73746218504955,0.186903956485225));
#12387=CARTESIAN_POINT('Ctrl Pts',(2.83764713126289,2.7316139424348,0.274001527981754));
#12388=CARTESIAN_POINT('Ctrl Pts',(2.82810498296568,2.72576546273895,0.360841618066086));
#12389=CARTESIAN_POINT('Ctrl Pts',(2.81441718411854,2.71991662923419,0.447018804472821));
#12390=CARTESIAN_POINT('Ctrl Pts',(2.79498016771151,2.71161113950106,0.569392562650119));
#12391=CARTESIAN_POINT('Ctrl Pts',(2.76718158097466,2.7033049363225,0.690428490885676));
#12392=CARTESIAN_POINT('Ctrl Pts',(2.73160210686119,2.69499768545555,0.809094381998766));
#12393=CARTESIAN_POINT('Ctrl Pts',(2.72542648768954,2.69355577494406,0.829691520389315));
#12394=CARTESIAN_POINT('Ctrl Pts',(2.71901656920653,2.69211383286841,0.850217300525002));
#12395=CARTESIAN_POINT('Ctrl Pts',(2.7123755330958,2.69067185748077,0.870666388989825));
#12396=CARTESIAN_POINT('Ctrl Pts',(2.67064740764895,2.68161138425584,0.999155696156249));
#12397=CARTESIAN_POINT('Ctrl Pts',(2.61979265389133,2.67255160135519,1.12463777940907));
#12398=CARTESIAN_POINT('Ctrl Pts',(2.56050167822933,2.66349257395265,1.24599674437055));
#12399=CARTESIAN_POINT('Ctrl Pts',(2.50071299431134,2.65435750204791,1.36837443702413));
#12400=CARTESIAN_POINT('Ctrl Pts',(2.43234529298495,2.64522319837834,1.48656062936928));
#12401=CARTESIAN_POINT('Ctrl Pts',(2.35605753556705,2.63608972977292,1.5993931294019));
#12402=CARTESIAN_POINT('Ctrl Pts',(2.30824860094078,2.63036585718514,1.67010436538998));
#12403=CARTESIAN_POINT('Ctrl Pts',(2.25732817701152,2.62464231256294,1.73871255946905));
#12404=CARTESIAN_POINT('Ctrl Pts',(2.20345030717718,2.61891911235483,1.80492507141801));
#12405=CARTESIAN_POINT('Ctrl Pts',(2.12615843289759,2.61070874931855,1.89991192158544));
#12406=CARTESIAN_POINT('Ctrl Pts',(2.04273521956806,2.60249780250347,1.99001459206904));
#12407=CARTESIAN_POINT('Ctrl Pts',(1.95373829132842,2.59428624309621,2.07422470903276));
#12408=CARTESIAN_POINT('Ctrl Pts',(1.91054670840689,2.59030104657237,2.11509317855876));
#12409=CARTESIAN_POINT('Ctrl Pts',(1.86604300917947,2.58631570576403,2.15457416437758));
#12410=CARTESIAN_POINT('Ctrl Pts',(1.8202943955014,2.58233021737761,2.19255519697283));
#12411=CARTESIAN_POINT('Ctrl Pts',(1.72604711272271,2.57411966364129,2.27080039024623));
#12412=CARTESIAN_POINT('Ctrl Pts',(1.62651467735229,2.56590848357433,2.34267673037767));
#12413=CARTESIAN_POINT('Ctrl Pts',(1.52277917244175,2.55769664838017,2.40780009086491));
#12414=CARTESIAN_POINT('Ctrl Pts',(1.47844499771388,2.55418709842765,2.43563232096971));
#12415=CARTESIAN_POINT('Ctrl Pts',(1.4333434682952,2.55067742881538,2.46223167461521));
#12416=CARTESIAN_POINT('Ctrl Pts',(1.38756025028133,2.54716763729551,2.4875707972306));
#12417=CARTESIAN_POINT('Ctrl Pts',(1.26891421197317,2.53807210235528,2.55323648529147));
#12418=CARTESIAN_POINT('Ctrl Pts',(1.14563385239945,2.52897755889248,2.61047602220136));
#12419=CARTESIAN_POINT('Ctrl Pts',(1.0189814365323,2.51988384752141,2.65889309143623));
#12420=CARTESIAN_POINT('Ctrl Pts',(0.892334871035826,2.5107905562101,2.70730792417368));
#12421=CARTESIAN_POINT('Ctrl Pts',(0.762315362595673,2.50169809691366,2.7469015143793));
#12422=CARTESIAN_POINT('Ctrl Pts',(0.630164154549595,2.49260631026847,2.77723091893705));
#12423=CARTESIAN_POINT('Ctrl Pts',(0.546879651692226,2.48687647289487,2.79634515495426));
#12424=CARTESIAN_POINT('Ctrl Pts',(0.462748127960112,2.48114690268412,2.81177890098223));
#12425=CARTESIAN_POINT('Ctrl Pts',(0.378079282353485,2.4754175597458,2.82341062940693));
#12426=CARTESIAN_POINT('Ctrl Pts',(0.255750957563129,2.46713988784921,2.84021598257331));
#12427=CARTESIAN_POINT('Ctrl Pts',(0.132273370076185,2.45886120387561,2.84908296321122));
#12428=CARTESIAN_POINT('Ctrl Pts',(0.00875639082543048,2.45058178679057,
2.84962297824459));
#12429=CARTESIAN_POINT('Ctrl Pts',(-0.0202735153242608,2.44863589479733,
2.84974989671226));
#12430=CARTESIAN_POINT('Ctrl Pts',(-0.0493055530627788,2.44668996230848,
2.84941707206123));
#12431=CARTESIAN_POINT('Ctrl Pts',(-0.0783252583048325,2.44474399294569,
2.84861987761965));
#12432=CARTESIAN_POINT('Ctrl Pts',(-0.201972236186597,2.43645261890334,
2.84522319654853));
#12433=CARTESIAN_POINT('Ctrl Pts',(-0.325394706421818,2.42816057543787,
2.83339201024013));
#12434=CARTESIAN_POINT('Ctrl Pts',(-0.447496781829693,2.41986814269175,
2.81355910618427));
#12435=CARTESIAN_POINT('Ctrl Pts',(-0.527029194075716,2.41446678339885,
2.80064074508239));
#12436=CARTESIAN_POINT('Ctrl Pts',(-0.606001457979839,2.4090652589459,2.78432861551543));
#12437=CARTESIAN_POINT('Ctrl Pts',(-0.684114254614127,2.40366364675096,
2.76475364718617));
#12438=CARTESIAN_POINT('Ctrl Pts',(-0.818136932673682,2.39439578587031,
2.73116773307915));
#12439=CARTESIAN_POINT('Ctrl Pts',(-0.949739937308827,2.38512918943378,
2.68795570610072));
#12440=CARTESIAN_POINT('Ctrl Pts',(-1.07763376262398,2.37586345593199,2.63566953190969));
#12441=CARTESIAN_POINT('Ctrl Pts',(-1.20431846106865,2.36668532202559,2.58387767883239));
#12442=CARTESIAN_POINT('Ctrl Pts',(-1.32736492605692,2.35750803481446,2.52318189258877));
#12443=CARTESIAN_POINT('Ctrl Pts',(-1.44550074330027,2.3483312040696,2.45407242604945));
#12444=CARTESIAN_POINT('Ctrl Pts',(-1.51594067256431,2.34285940623877,2.41286505940909));
#12445=CARTESIAN_POINT('Ctrl Pts',(-1.58463427958763,2.33738777069478,2.36866554426707));
#12446=CARTESIAN_POINT('Ctrl Pts',(-1.65130600877161,2.33191621471365,2.32157107421747));
#12447=CARTESIAN_POINT('Ctrl Pts',(-1.75184851670552,2.32366498188413,2.25055152535383));
#12448=CARTESIAN_POINT('Ctrl Pts',(-1.84777688142223,2.31541235096666,2.17295356714672));
#12449=CARTESIAN_POINT('Ctrl Pts',(-1.9380254250103,2.30715890415833,2.08921697074446));
#12450=CARTESIAN_POINT('Ctrl Pts',(-2.03126753674888,2.2986316883282,2.00270280920868));
#12451=CARTESIAN_POINT('Ctrl Pts',(-2.11844575454504,2.29010360158284,1.90963650255824));
#12452=CARTESIAN_POINT('Ctrl Pts',(-2.19898427330714,2.28157528599718,1.81115156281633));
#12453=CARTESIAN_POINT('Ctrl Pts',(-2.26639938968078,2.27443662245438,1.72871431693944));
#12454=CARTESIAN_POINT('Ctrl Pts',(-2.32916283406357,2.26729779857235,1.64248150554385));
#12455=CARTESIAN_POINT('Ctrl Pts',(-2.38696115341166,2.26015919092189,1.55313203489346));
#12456=CARTESIAN_POINT('Ctrl Pts',(-2.46323386771049,2.2507388308153,1.43522330113557));
#12457=CARTESIAN_POINT('Ctrl Pts',(-2.53094821808017,2.24131998429432,1.31176553557256));
#12458=CARTESIAN_POINT('Ctrl Pts',(-2.58945805705541,2.23190201879764,1.18408840259321));
#12459=CARTESIAN_POINT('Ctrl Pts',(-2.64684412511343,2.2226649397281,1.05886350416706));
#12460=CARTESIAN_POINT('Ctrl Pts',(-2.69537627053228,2.21342870816502,0.929578579642012));
#12461=CARTESIAN_POINT('Ctrl Pts',(-2.73439894914873,2.20419272729932,0.797471141416176));
#12462=CARTESIAN_POINT('Ctrl Pts',(-2.75662093382076,2.19893317484148,0.722240799179309));
#12463=CARTESIAN_POINT('Ctrl Pts',(-2.77575823263306,2.19367370368192,0.646094931826458));
#12464=CARTESIAN_POINT('Ctrl Pts',(-2.79168214922777,2.18841420360768,0.56926171586123));
#12465=CARTESIAN_POINT('Ctrl Pts',(-2.81069174901636,2.18213553523456,0.477540016787891));
#12466=CARTESIAN_POINT('Ctrl Pts',(-2.82511457512874,2.17585595672354,0.384865577083334));
#12467=CARTESIAN_POINT('Ctrl Pts',(-2.83472867179422,2.1695758005696,0.291690675508813));
#12468=CARTESIAN_POINT('Ctrl Pts',(-2.84825497168096,2.16074010040666,0.160600703724005));
#12469=CARTESIAN_POINT('Ctrl Pts',(-2.85226036880898,2.15190325683758,0.028520551691609));
#12470=CARTESIAN_POINT('Ctrl Pts',(-2.84707363368557,2.14306619583182,-0.103208249395973));
#12471=CARTESIAN_POINT('Ctrl Pts',(-2.84190671011819,2.13426288937977,-0.234433891470715));
#12472=CARTESIAN_POINT('Ctrl Pts',(-2.827618090831,2.12545936714896,-0.365309681728793));
#12473=CARTESIAN_POINT('Ctrl Pts',(-2.80458334954684,2.11665654453875,-0.494518897726551));
#12474=CARTESIAN_POINT('',(-2.11596363778888,2.11666666302544,-0.373098825439504));
#12475=CARTESIAN_POINT('Ctrl Pts',(-2.11596363778888,2.11666666302544,-0.373098825439504));
#12476=CARTESIAN_POINT('Ctrl Pts',(-2.11596363651329,2.11665130912368,-0.37309881786039));
#12477=CARTESIAN_POINT('Ctrl Pts',(-2.1159636365634,2.11663595520812,-0.373098810515882));
#12478=CARTESIAN_POINT('Ctrl Pts',(-2.11596363793934,2.11662060127888,-0.373098803405978));
#12479=CARTESIAN_POINT('Ctrl Pts',(-2.11596683312042,2.08096600528101,-0.373082292924252));
#12480=CARTESIAN_POINT('Ctrl Pts',(-2.12311934727396,2.0452337361124,-0.374330868757299));
#12481=CARTESIAN_POINT('Ctrl Pts',(-2.13605487204922,2.01089616470858,-0.376602271121508));
#12482=CARTESIAN_POINT('Ctrl Pts',(-2.14744386484174,1.98066388886159,-0.378602111530333));
#12483=CARTESIAN_POINT('Ctrl Pts',(-2.16331663724392,1.95151252630738,-0.38139500483258));
#12484=CARTESIAN_POINT('Ctrl Pts',(-2.18273341382768,1.92448634192568,-0.384814546287745));
#12485=CARTESIAN_POINT('Ctrl Pts',(-2.19478368808634,1.90771358190755,-0.386936752937024));
#12486=CARTESIAN_POINT('Ctrl Pts',(-2.20819877256644,1.89176014158068,-0.389300287494568));
#12487=CARTESIAN_POINT('Ctrl Pts',(-2.22275031585101,1.87688528762621,-0.391864731679025));
#12488=CARTESIAN_POINT('Ctrl Pts',(-2.22303912351179,1.87659006314788,-0.391915628763385));
#12489=CARTESIAN_POINT('Ctrl Pts',(-2.22332838298208,1.87629525933482,-0.391966606159889));
#12490=CARTESIAN_POINT('Ctrl Pts',(-2.22361809235949,1.87600087842983,-0.392017663531752));
#12491=CARTESIAN_POINT('Ctrl Pts',(-2.24414409427434,1.85514389729317,-0.395635094634655));
#12492=CARTESIAN_POINT('Ctrl Pts',(-2.26693329697911,1.83641063434651,-0.399654824590917));
#12493=CARTESIAN_POINT('Ctrl Pts',(-2.29128006082217,1.82059521922762,-0.403951952341833));
#12494=CARTESIAN_POINT('Ctrl Pts',(-2.31715625200098,1.80378630335581,-0.408519019239073));
#12495=CARTESIAN_POINT('Ctrl Pts',(-2.34479013883076,1.79027596583773,-0.413399137995121));
#12496=CARTESIAN_POINT('Ctrl Pts',(-2.37328386590736,1.78098419803457,-0.418433352695355));
#12497=CARTESIAN_POINT('Ctrl Pts',(-2.39813004265473,1.77288189170896,-0.422823125500084));
#12498=CARTESIAN_POINT('Ctrl Pts',(-2.42362820852464,1.76798772624127,-0.427329750155805));
#12499=CARTESIAN_POINT('Ctrl Pts',(-2.44917202781645,1.76686823687416,-0.431845791537889));
#12500=CARTESIAN_POINT('Ctrl Pts',(-2.45292199576584,1.76670388990637,-0.432508770329255));
#12501=CARTESIAN_POINT('Ctrl Pts',(-2.4566729502669,1.766620801847,-0.433171952337485));
#12502=CARTESIAN_POINT('Ctrl Pts',(-2.460422980835,1.76662066484191,-0.433834998833824));
#12503=CARTESIAN_POINT('Ctrl Pts',(-2.46095539978625,1.76662064539031,-0.433929136338518));
#12504=CARTESIAN_POINT('Ctrl Pts',(-2.46148780012147,1.76662229797987,-0.434023271112983));
#12505=CARTESIAN_POINT('Ctrl Pts',(-2.46202017631675,1.7666256170716,-0.434117402177783));
#12506=CARTESIAN_POINT('Ctrl Pts',(-2.49337021729807,1.76682106845124,-0.439660498892463));
#12507=CARTESIAN_POINT('Ctrl Pts',(-2.52470190520736,1.77280099958023,-0.445197320624149));
#12508=CARTESIAN_POINT('Ctrl Pts',(-2.55492178827082,1.78347584413678,-0.450535391174815));
#12509=CARTESIAN_POINT('Ctrl Pts',(-2.57526760252786,1.79066278142951,-0.454129296276524));
#12510=CARTESIAN_POINT('Ctrl Pts',(-2.59510952423172,1.79997638628388,-0.457633124067283));
#12511=CARTESIAN_POINT('Ctrl Pts',(-2.61412174689286,1.81107368218895,-0.460989551695197));
#12512=CARTESIAN_POINT('Ctrl Pts',(-2.64023837149477,1.8263177657669,-0.465600194118444));
#12513=CARTESIAN_POINT('Ctrl Pts',(-2.66478693875802,1.8449270679929,-0.46993226175055));
#12514=CARTESIAN_POINT('Ctrl Pts',(-2.6870038349963,1.8660042935492,-0.47385152302486));
#12515=CARTESIAN_POINT('Ctrl Pts',(-2.69130665910911,1.87008639364914,-0.474610580083713));
#12516=CARTESIAN_POINT('Ctrl Pts',(-2.69552217701995,1.87426106856329,-0.475354180395831));
#12517=CARTESIAN_POINT('Ctrl Pts',(-2.6996450775538,1.87852182289951,-0.476081390939429));
#12518=CARTESIAN_POINT('Ctrl Pts',(-2.71349628945441,1.89283616560143,-0.478524512536237));
#12519=CARTESIAN_POINT('Ctrl Pts',(-2.72630673440351,1.90812665369922,-0.48078284574271));
#12520=CARTESIAN_POINT('Ctrl Pts',(-2.73788531809392,1.9241607224898,-0.482822724168243));
#12521=CARTESIAN_POINT('Ctrl Pts',(-2.75564388146651,1.94875285174769,-0.485951371959786));
#12522=CARTESIAN_POINT('Ctrl Pts',(-2.77050254115736,1.97509252268725,-0.488565753139015));
#12523=CARTESIAN_POINT('Ctrl Pts',(-2.78163830746197,2.00236904489192,-0.490520971618943));
#12524=CARTESIAN_POINT('Ctrl Pts',(-2.79136325815834,2.02618984234338,-0.492228479014286));
#12525=CARTESIAN_POINT('Ctrl Pts',(-2.79824948844992,2.05072567441806,-0.49343337360953));
#12526=CARTESIAN_POINT('Ctrl Pts',(-2.80177308229317,2.07545781701756,-0.494043524091528));
#12527=CARTESIAN_POINT('Ctrl Pts',(-2.80372504497939,2.08915866383823,-0.494381528704665));
#12528=CARTESIAN_POINT('Ctrl Pts',(-2.80464571747422,2.10292010438476,-0.494537132455511));
#12529=CARTESIAN_POINT('Ctrl Pts',(-2.80458334954684,2.11665654453875,-0.494518897726551));
#12530=CARTESIAN_POINT('Ctrl Pts',(2.14860532739796,6.34999974434397,2.61193398279736E-6));
#12531=CARTESIAN_POINT('Ctrl Pts',(2.14880376471062,6.340662649241,0.105046613947578));
#12532=CARTESIAN_POINT('Ctrl Pts',(2.14144274304709,6.33132557235638,0.210199967010338));
#12533=CARTESIAN_POINT('Ctrl Pts',(2.12639571524597,6.32198850691087,0.314230311092142));
#12534=CARTESIAN_POINT('Ctrl Pts',(2.11302081122913,6.31368903702332,0.406700125418489));
#12535=CARTESIAN_POINT('Ctrl Pts',(2.09357387058337,6.30538957617378,0.498281788208163));
#12536=CARTESIAN_POINT('Ctrl Pts',(2.06800062383508,6.29709011960108,0.588110040716897));
#12537=CARTESIAN_POINT('Ctrl Pts',(2.04328873085351,6.28907020391933,0.67491271323503));
#12538=CARTESIAN_POINT('Ctrl Pts',(2.01285670810749,6.28105029223114,0.760077599724587));
#12539=CARTESIAN_POINT('Ctrl Pts',(1.97717697406473,6.27303038024048,0.842964335289945));
#12540=CARTESIAN_POINT('Ctrl Pts',(1.93376225290463,6.26327183657012,0.943820034161666));
#12541=CARTESIAN_POINT('Ctrl Pts',(1.88259112117066,6.2535132075724,1.04129200227137));
#12542=CARTESIAN_POINT('Ctrl Pts',(1.82444223822442,6.24375455353849,1.13440813463617));
#12543=CARTESIAN_POINT('Ctrl Pts',(1.76550266292752,6.23386320403898,1.22879043429179));
#12544=CARTESIAN_POINT('Ctrl Pts',(1.69939356847182,6.22397182881777,1.31869878887616));
#12545=CARTESIAN_POINT('Ctrl Pts',(1.62687779287196,6.21408049065924,1.40309928835906));
#12546=CARTESIAN_POINT('Ctrl Pts',(1.58284130110669,6.20807380000796,1.45435298963604));
#12547=CARTESIAN_POINT('Ctrl Pts',(1.53644130771525,6.20206712302445,1.50357504259231));
#12548=CARTESIAN_POINT('Ctrl Pts',(1.48784192275397,6.19606047376889,1.55052731215525));
#12549=CARTESIAN_POINT('Ctrl Pts',(1.41581017995234,6.18715769825804,1.62011777729805));
#12550=CARTESIAN_POINT('Ctrl Pts',(1.33889901588293,6.17825493322457,1.68476045955435));
#12551=CARTESIAN_POINT('Ctrl Pts',(1.2577527291572,6.16935216964046,1.74355725382114));
#12552=CARTESIAN_POINT('Ctrl Pts',(1.22781639563224,6.1660677790577,1.76524845516124));
#12553=CARTESIAN_POINT('Ctrl Pts',(1.19730405087015,6.16278338867221,1.78614435142343));
#12554=CARTESIAN_POINT('Ctrl Pts',(1.16624930383038,6.15949899803066,1.80620114089016));
#12555=CARTESIAN_POINT('Ctrl Pts',(1.08206834466982,6.15059590974889,1.8605696331799));
#12556=CARTESIAN_POINT('Ctrl Pts',(0.993900225083129,6.14169281958567,1.90876882406862));
#12557=CARTESIAN_POINT('Ctrl Pts',(0.902819134132778,6.13278971851196,1.95055782333801));
#12558=CARTESIAN_POINT('Ctrl Pts',(0.856105440240191,6.12822349369061,1.97199057627915));
#12559=CARTESIAN_POINT('Ctrl Pts',(0.808625878921926,6.12365726599931,1.99173792876364));
#12560=CARTESIAN_POINT('Ctrl Pts',(0.760526869968194,6.11909103421993,2.00977246655487));
#12561=CARTESIAN_POINT('Ctrl Pts',(0.653502716799387,6.10893080223198,2.0499007597751));
#12562=CARTESIAN_POINT('Ctrl Pts',(0.543315077176724,6.09877051545036,2.08159140603936));
#12563=CARTESIAN_POINT('Ctrl Pts',(0.431339421902752,6.08861022307749,2.10457030743763));
#12564=CARTESIAN_POINT('Ctrl Pts',(0.320792725181825,6.07857958957245,2.12725596743792));
#12565=CARTESIAN_POINT('Ctrl Pts',(0.208501993543669,6.06854895061798,2.14145099637505));
#12566=CARTESIAN_POINT('Ctrl Pts',(0.0957817413243718,6.05851835355675,
2.14684298427428));
#12567=CARTESIAN_POINT('Ctrl Pts',(0.034359674707909,6.05305260992357,2.14978111680522));
#12568=CARTESIAN_POINT('Ctrl Pts',(-0.0271899640555367,6.04758687872947,
2.15010455086845));
#12569=CARTESIAN_POINT('Ctrl Pts',(-0.0886534609856654,6.04212116763432,
2.14775622505523));
#12570=CARTESIAN_POINT('Ctrl Pts',(-0.16441281023487,6.03538418167625,2.14486169994162));
#12571=CARTESIAN_POINT('Ctrl Pts',(-0.24001500802354,6.02864720091353,2.13790744511307));
#12572=CARTESIAN_POINT('Ctrl Pts',(-0.315006532193144,6.021910216931,2.12679827092486));
#12573=CARTESIAN_POINT('Ctrl Pts',(-0.424539553847577,6.01207014206099,
2.1105721516348));
#12574=CARTESIAN_POINT('Ctrl Pts',(-0.532768639141451,6.00223006032192,
2.08547983748586));
#12575=CARTESIAN_POINT('Ctrl Pts',(-0.63842842684824,5.99238994549198,2.05221400133585));
#12576=CARTESIAN_POINT('Ctrl Pts',(-0.735920068252026,5.98331053158066,
2.0215198173012));
#12577=CARTESIAN_POINT('Ctrl Pts',(-0.831223638478912,5.97423108949699,
1.9838679974274));
#12578=CARTESIAN_POINT('Ctrl Pts',(-0.92336388243848,5.96515159864248,1.93983728460326));
#12579=CARTESIAN_POINT('Ctrl Pts',(-1.05354848936501,5.9523232198886,1.87762645472721));
#12580=CARTESIAN_POINT('Ctrl Pts',(-1.17769422010297,5.93949491342787,1.80256132904901));
#12581=CARTESIAN_POINT('Ctrl Pts',(-1.2932278247383,5.92666663225393,1.71602372051491));
#12582=CARTESIAN_POINT('Ctrl Pts',(-1.40034941353704,5.91477237979598,1.63578692580678));
#12583=CARTESIAN_POINT('Ctrl Pts',(-1.50006803701196,5.90287814907656,1.54568645828586));
#12584=CARTESIAN_POINT('Ctrl Pts',(-1.59029140712846,5.89098390262751,1.44680014240826));
#12585=CARTESIAN_POINT('Ctrl Pts',(-1.59737644411084,5.89004987438338,1.43903482390886));
#12586=CARTESIAN_POINT('Ctrl Pts',(-1.60440290204282,5.88911584604226,1.43121531786644));
#12587=CARTESIAN_POINT('Ctrl Pts',(-1.61136975410245,5.88818181758599,1.42334214208012));
#12588=CARTESIAN_POINT('Ctrl Pts',(-1.62094055997566,5.88689868354518,1.4125262619076));
#12589=CARTESIAN_POINT('Ctrl Pts',(-1.63039714217838,5.88561554994813,1.40161105365249));
#12590=CARTESIAN_POINT('Ctrl Pts',(-1.63973690885178,5.88433241671821,1.39059802595259));
#12591=CARTESIAN_POINT('Ctrl Pts',(-1.75049262821925,5.86911636808519,1.25999992345493));
#12592=CARTESIAN_POINT('Ctrl Pts',(-1.84481868938701,5.85390037108115,1.11564909326681));
#12593=CARTESIAN_POINT('Ctrl Pts',(-1.92110731644144,5.83868429795035,0.962331968016694));
#12594=CARTESIAN_POINT('Ctrl Pts',(-1.96701951219276,5.82952692607041,0.870062305574195));
#12595=CARTESIAN_POINT('Ctrl Pts',(-2.00639931667232,5.8203695266181,0.774544462738395));
#12596=CARTESIAN_POINT('Ctrl Pts',(-2.03890199800151,5.81121207174598,0.676814504551522));
#12597=CARTESIAN_POINT('Ctrl Pts',(-2.07883143620631,5.79996216824644,0.556753569065732));
#12598=CARTESIAN_POINT('Ctrl Pts',(-2.1084572478166,5.78871235944162,0.433114934641564));
#12599=CARTESIAN_POINT('Ctrl Pts',(-2.12702197944784,5.77746258842401,0.307856734199112));
#12600=CARTESIAN_POINT('Ctrl Pts',(-2.14391388897004,5.76722650648383,0.193885240788101));
#12601=CARTESIAN_POINT('Ctrl Pts',(-2.15164844402679,5.75699045582787,0.0785742535437493));
#12602=CARTESIAN_POINT('Ctrl Pts',(-2.14968871231329,5.74675439358754,-0.036584698704585));
#12603=CARTESIAN_POINT('Ctrl Pts',(-2.14889022610864,5.74258374388453,-0.0835058328982378));
#12604=CARTESIAN_POINT('Ctrl Pts',(-2.14648276546956,5.73841309225837,-0.130401630189374));
#12605=CARTESIAN_POINT('Ctrl Pts',(-2.14250453145903,5.73424243580935,-0.17717227139658));
#12606=CARTESIAN_POINT('Ctrl Pts',(-2.13253902319035,5.72379490778094,-0.294333104683244));
#12607=CARTESIAN_POINT('Ctrl Pts',(-2.11273259117636,5.71334734433916,-0.410580783624014));
#12608=CARTESIAN_POINT('Ctrl Pts',(-2.08371969928467,5.70289976543379,-0.524488619165007));
#12609=CARTESIAN_POINT('Ctrl Pts',(-2.05374754544138,5.69210675509167,-0.64216262365711));
#12610=CARTESIAN_POINT('Ctrl Pts',(-2.01394981846877,5.68131372824648,-0.757340867267386));
#12611=CARTESIAN_POINT('Ctrl Pts',(-1.96497129776221,5.67052070689296,-0.868449422790271));
#12612=CARTESIAN_POINT('Ctrl Pts',(-1.94493138059279,5.66610466388447,-0.91391029456369));
#12613=CARTESIAN_POINT('Ctrl Pts',(-1.92335391171395,5.66168862179535,-0.958689730844809));
#12614=CARTESIAN_POINT('Ctrl Pts',(-1.90028070903563,5.65727258213216,-1.00267903367898));
#12615=CARTESIAN_POINT('Ctrl Pts',(-1.85254375919245,5.6481360844016,-1.09369002908814));
#12616=CARTESIAN_POINT('Ctrl Pts',(-1.79834239655419,5.63899961794059,-1.18142666041962));
#12617=CARTESIAN_POINT('Ctrl Pts',(-1.73808607165971,5.6298631690235,-1.26478002970971));
#12618=CARTESIAN_POINT('Ctrl Pts',(-1.69259856836636,5.6229660631855,-1.32770349320893));
#12619=CARTESIAN_POINT('Ctrl Pts',(-1.64366163074749,5.61606896734535,-1.38812906495699));
#12620=CARTESIAN_POINT('Ctrl Pts',(-1.59146897410807,5.60917187559826,-1.44558863599498));
#12621=CARTESIAN_POINT('Ctrl Pts',(-1.52248449585653,5.60005579861998,-1.52153454072249));
#12622=CARTESIAN_POINT('Ctrl Pts',(-1.44781169944092,5.59093972879212,-1.59229708604899));
#12623=CARTESIAN_POINT('Ctrl Pts',(-1.36849398618179,5.58182365248058,-1.65734003225809));
#12624=CARTESIAN_POINT('Ctrl Pts',(-1.36408398969738,5.58131680649582,-1.66095636399952));
#12625=CARTESIAN_POINT('Ctrl Pts',(-1.35965964204295,5.58080996049102,-1.66455502598097));
#12626=CARTESIAN_POINT('Ctrl Pts',(-1.355221125012,5.58030311446383,-1.66813593002742));
#12627=CARTESIAN_POINT('Ctrl Pts',(-1.269060793176,5.57046423774273,-1.73764830967226));
#12628=CARTESIAN_POINT('Ctrl Pts',(-1.17755335950336,5.56062527924614,-1.80048101079417));
#12629=CARTESIAN_POINT('Ctrl Pts',(-1.08184958870044,5.55078630172061,-1.85609286767396));
#12630=CARTESIAN_POINT('Ctrl Pts',(-0.985603365185632,5.54089155648608,
-1.9120199347312));
#12631=CARTESIAN_POINT('Ctrl Pts',(-0.885111900569775,5.53099679200629,
-1.96064473276489));
#12632=CARTESIAN_POINT('Ctrl Pts',(-0.781515883586216,5.5211020721009,-2.00137462967412));
#12633=CARTESIAN_POINT('Ctrl Pts',(-0.719503403348289,5.51517910188969,
-2.02575550840595));
#12634=CARTESIAN_POINT('Ctrl Pts',(-0.656378011428396,5.50925614765042,
-2.04730662538622));
#12635=CARTESIAN_POINT('Ctrl Pts',(-0.592382047293052,5.50333322307176,
-2.06589217974674));
#12636=CARTESIAN_POINT('Ctrl Pts',(-0.495077335604388,5.49432752284883,
-2.09415118065497));
#12637=CARTESIAN_POINT('Ctrl Pts',(-0.395728162407976,5.48532182713199,
-2.11555758228668));
#12638=CARTESIAN_POINT('Ctrl Pts',(-0.295343829160877,5.47631612587051,
-2.12958822780567));
#12639=CARTESIAN_POINT('Ctrl Pts',(-0.277744101562778,5.47473721525861,
-2.13204812897922));
#12640=CARTESIAN_POINT('Ctrl Pts',(-0.260112597674987,5.47315830447628,
-2.13428143399914));
#12641=CARTESIAN_POINT('Ctrl Pts',(-0.242454802330516,5.47157939346935,
-2.13628548398197));
#12642=CARTESIAN_POINT('Ctrl Pts',(-0.141589680320261,5.46256031445918,
-2.14773304819311));
#12643=CARTESIAN_POINT('Ctrl Pts',(-0.0398667183094937,5.45354122812046,
-2.15169583131827));
#12644=CARTESIAN_POINT('Ctrl Pts',(0.0616071250593509,5.44452212435753,
-2.14844214333508));
#12645=CARTESIAN_POINT('Ctrl Pts',(0.129706859397744,5.43846934711135,-2.14625857287082));
#12646=CARTESIAN_POINT('Ctrl Pts',(0.197694264497796,5.43241656201761,-2.14082596253566));
#12647=CARTESIAN_POINT('Ctrl Pts',(0.265237158184707,5.42636376602485,-2.13223832829264));
#12648=CARTESIAN_POINT('Ctrl Pts',(0.382371048324121,5.41586691724992,-2.11734552534815));
#12649=CARTESIAN_POINT('Ctrl Pts',(0.49831454004301,5.40537003965045,-2.09295237197418));
#12650=CARTESIAN_POINT('Ctrl Pts',(0.611562267195913,5.39487316597188,-2.0594489299804));
#12651=CARTESIAN_POINT('Ctrl Pts',(0.722308338854742,5.38460816945648,-2.02668558292576));
#12652=CARTESIAN_POINT('Ctrl Pts',(0.830477706126031,5.37434317669068,-1.98520949062172));
#12653=CARTESIAN_POINT('Ctrl Pts',(0.93464491267495,5.36407821829738,-1.9353401923379));
#12654=CARTESIAN_POINT('Ctrl Pts',(0.984316346245632,5.35918344175655,-1.91156035203127));
#12655=CARTESIAN_POINT('Ctrl Pts',(1.03307739142291,5.35428867303132,-1.88587144447327));
#12656=CARTESIAN_POINT('Ctrl Pts',(1.08077076705523,5.34939391544197,-1.85830486182312));
#12657=CARTESIAN_POINT('Ctrl Pts',(1.13078671291648,5.34426079312997,-1.82939584275852));
#12658=CARTESIAN_POINT('Ctrl Pts',(1.17960617224486,5.33912767551624,-1.79843411893778));
#12659=CARTESIAN_POINT('Ctrl Pts',(1.2270341705754,5.3339945580915,-1.76547079971493));
#12660=CARTESIAN_POINT('Ctrl Pts',(1.32471108062967,5.3234230166678,-1.69758357528728));
#12661=CARTESIAN_POINT('Ctrl Pts',(1.41648363708775,5.31285147604563,-1.62120442851145));
#12662=CARTESIAN_POINT('Ctrl Pts',(1.50135016528333,5.30227989683554,-1.53778457154753));
#12663=CARTESIAN_POINT('Ctrl Pts',(1.58124141099987,5.29232807424726,-1.45925518626405));
#12664=CARTESIAN_POINT('Ctrl Pts',(1.65501230994021,5.28237621746289,-1.37448765350144));
#12665=CARTESIAN_POINT('Ctrl Pts',(1.72186324495689,5.27242429362231,-1.28471467058922));
#12666=CARTESIAN_POINT('Ctrl Pts',(1.81836964190101,5.25805763873146,-1.15511787255459));
#12667=CARTESIAN_POINT('Ctrl Pts',(1.90070202076568,5.24369111383716,-1.01477291661791));
#12668=CARTESIAN_POINT('Ctrl Pts',(1.96642481069052,5.22932461427314,-0.867071437992345));
#12669=CARTESIAN_POINT('Ctrl Pts',(2.01660616146925,5.21835535452459,-0.754296862872764));
#12670=CARTESIAN_POINT('Ctrl Pts',(2.05710374954887,5.20738610954305,-0.637233730207292));
#12671=CARTESIAN_POINT('Ctrl Pts',(2.08681487532426,5.19641683273928,-0.517400885311197));
#12672=CARTESIAN_POINT('Ctrl Pts',(2.08768368483754,5.19609607033825,-0.513896746274617));
#12673=CARTESIAN_POINT('Ctrl Pts',(2.08854326971608,5.19577530791001,-0.510390239614455));
#12674=CARTESIAN_POINT('Ctrl Pts',(2.08939363433078,5.19545454545339,-0.506881411421222));
#12675=CARTESIAN_POINT('Ctrl Pts',(2.12478138995841,5.18210607912133,-0.360862218600595));
#12676=CARTESIAN_POINT('Ctrl Pts',(2.14413645684879,5.16875764625848,-0.211109615031524));
#12677=CARTESIAN_POINT('Ctrl Pts',(2.14794363642467,5.15540918199055,-0.06094667525413));
#12678=CARTESIAN_POINT('Ctrl Pts',(2.15145408794799,5.14310108467356,0.0775127039739754));
#12679=CARTESIAN_POINT('Ctrl Pts',(2.14174521530511,5.13079296065605,0.216322310287955));
#12680=CARTESIAN_POINT('Ctrl Pts',(2.11916587699683,5.11848475908094,0.35290065136281));
#12681=CARTESIAN_POINT('Ctrl Pts',(2.10039841736405,5.10825444705588,0.46642162650563));
#12682=CARTESIAN_POINT('Ctrl Pts',(2.07270108649064,5.09802420591568,0.578596776354617));
#12683=CARTESIAN_POINT('Ctrl Pts',(2.03621821645373,5.0877939988326,0.687825029565731));
#12684=CARTESIAN_POINT('Ctrl Pts',(2.00179883488851,5.07814241712515,0.790875280852756));
#12685=CARTESIAN_POINT('Ctrl Pts',(1.95956019064648,5.06849086573123,0.891301421975115));
#12686=CARTESIAN_POINT('Ctrl Pts',(1.90966579129595,5.05883931372533,0.987763415838006));
#12687=CARTESIAN_POINT('Ctrl Pts',(1.87981301268525,5.05306460455893,1.04547848174961));
#12688=CARTESIAN_POINT('Ctrl Pts',(1.84722039009149,5.04728989517344,1.1017746186486));
#12689=CARTESIAN_POINT('Ctrl Pts',(1.81210119078509,5.04151517894493,1.15645675235276));
#12690=CARTESIAN_POINT('Ctrl Pts',(1.75066236072355,5.03141267615376,1.25211970556366));
#12691=CARTESIAN_POINT('Ctrl Pts',(1.68154128808941,5.02131011601506,1.34277513267819));
#12692=CARTESIAN_POINT('Ctrl Pts',(1.60581470583693,5.01120753771401,1.42753203538759));
#12693=CARTESIAN_POINT('Ctrl Pts',(1.52826415897905,5.0008616268249,1.51433040868771));
#12694=CARTESIAN_POINT('Ctrl Pts',(1.443785182022,4.99051569688795,1.59494374835389));
#12695=CARTESIAN_POINT('Ctrl Pts',(1.35348823723746,4.98016978998863,1.66838712784109));
#12696=CARTESIAN_POINT('Ctrl Pts',(1.30803241324631,4.97496162127189,1.70535880323111));
#12697=CARTESIAN_POINT('Ctrl Pts',(1.26110159502111,4.96975345839323,1.74051296377186));
#12698=CARTESIAN_POINT('Ctrl Pts',(1.21283431888366,4.96454530672151,1.7737200509744));
#12699=CARTESIAN_POINT('Ctrl Pts',(1.12974779416806,4.9555800769173,1.83088220497145));
#12700=CARTESIAN_POINT('Ctrl Pts',(1.04261723061714,4.94661486682201,1.88232639240326));
#12701=CARTESIAN_POINT('Ctrl Pts',(0.952263314461416,4.93764966669292,1.92728410921836));
#12702=CARTESIAN_POINT('Ctrl Pts',(0.897179510252508,4.93218407815381,1.95469235200503));
#12703=CARTESIAN_POINT('Ctrl Pts',(0.840898457955948,4.92671849331882,1.97969045585849));
#12704=CARTESIAN_POINT('Ctrl Pts',(0.783611574738666,4.92125290998036,2.00211210972785));
#12705=CARTESIAN_POINT('Ctrl Pts',(0.689741169800707,4.91229699385456,2.0388522779809));
#12706=CARTESIAN_POINT('Ctrl Pts',(0.593169828820591,4.90334108174698,2.06867185494086));
#12707=CARTESIAN_POINT('Ctrl Pts',(0.495016264703413,4.89438516394511,2.09155192935259));
#12708=CARTESIAN_POINT('Ctrl Pts',(0.470140463553974,4.89211539786627,2.0973505998998));
#12709=CARTESIAN_POINT('Ctrl Pts',(0.445163078199004,4.88984563142169,2.10270380045615));
#12710=CARTESIAN_POINT('Ctrl Pts',(0.420102366121439,4.88757586445325,2.10761174972201));
#12711=CARTESIAN_POINT('Ctrl Pts',(0.310810276068341,4.87767720015569,2.12901577174183));
#12712=CARTESIAN_POINT('Ctrl Pts',(0.199882936393077,4.86777845891062,2.14196622068233));
#12713=CARTESIAN_POINT('Ctrl Pts',(0.0886129714964294,4.85787970263818,
2.14648118705205));
#12714=CARTESIAN_POINT('Ctrl Pts',(-0.022450796580891,4.84799928996872,
2.15098778663828));
#12715=CARTESIAN_POINT('Ctrl Pts',(-0.13385729235645,4.83811886232756,2.14709013848741));
#12716=CARTESIAN_POINT('Ctrl Pts',(-0.24432546663264,4.82823848129131,2.13475568838697));
#12717=CARTESIAN_POINT('Ctrl Pts',(-0.310039445163978,4.82236095908592,
2.12741831910024));
#12718=CARTESIAN_POINT('Ctrl Pts',(-0.375421367891689,4.81648345337251,
2.11709447375088));
#12719=CARTESIAN_POINT('Ctrl Pts',(-0.440199281626035,4.81060597711322,
2.10376877792093));
#12720=CARTESIAN_POINT('Ctrl Pts',(-0.539190248072235,4.80162425754816,
2.08340499290951));
#12721=CARTESIAN_POINT('Ctrl Pts',(-0.636768480871051,4.79264254195598,
2.05602620706925));
#12722=CARTESIAN_POINT('Ctrl Pts',(-0.731816032994038,4.7836608170803,2.02161947317196));
#12723=CARTESIAN_POINT('Ctrl Pts',(-0.829615042770138,4.77441908723767,
1.98621672549856));
#12724=CARTESIAN_POINT('Ctrl Pts',(-0.924733513944005,4.76517734756626,
1.94337333383143));
#12725=CARTESIAN_POINT('Ctrl Pts',(-1.01624004259855,4.75593558362472,1.89387054506982));
#12726=CARTESIAN_POINT('Ctrl Pts',(-1.08983740092588,4.74850256849036,1.85405617842014));
#12727=CARTESIAN_POINT('Ctrl Pts',(-1.16109841751715,4.7410695376563,1.80993521110809));
#12728=CARTESIAN_POINT('Ctrl Pts',(-1.22955343864502,4.73363648360911,1.76193346081459));
#12729=CARTESIAN_POINT('Ctrl Pts',(-1.3313510344479,4.72258299156411,1.69055136650364));
#12730=CARTESIAN_POINT('Ctrl Pts',(-1.4271061270336,4.71152950431796,1.61048339724775));
#12731=CARTESIAN_POINT('Ctrl Pts',(-1.51542254683858,4.70047603071412,1.52291719146958));
#12732=CARTESIAN_POINT('Ctrl Pts',(-1.6008248474513,4.68978728135569,1.43824035056166));
#12733=CARTESIAN_POINT('Ctrl Pts',(-1.67927212165502,4.67909854475413,1.34655087460194));
#12734=CARTESIAN_POINT('Ctrl Pts',(-1.74946300834417,4.66840982890598,1.24889502111413));
#12735=CARTESIAN_POINT('Ctrl Pts',(-1.77516813001075,4.66449543553818,1.21313175163907));
#12736=CARTESIAN_POINT('Ctrl Pts',(-1.79976549737413,4.66058104495373,1.17656810305738));
#12737=CARTESIAN_POINT('Ctrl Pts',(-1.82318948990156,4.65666665754538,1.13925490583306));
#12738=CARTESIAN_POINT('Ctrl Pts',(-1.84430714638878,4.65313768234824,1.10561558151633));
#12739=CARTESIAN_POINT('Ctrl Pts',(-1.86446248188883,4.64960871019584,1.0713806031278));
#12740=CARTESIAN_POINT('Ctrl Pts',(-1.88360724270868,4.6460797394394,1.03659237669773));
#12741=CARTESIAN_POINT('Ctrl Pts',(-1.94789431407824,4.63422964650719,0.919775393901501));
#12742=CARTESIAN_POINT('Ctrl Pts',(-2.00078253174395,4.62237956931563,0.796719402573613));
#12743=CARTESIAN_POINT('Ctrl Pts',(-2.04194024364151,4.61052944543686,0.669845135897601));
#12744=CARTESIAN_POINT('Ctrl Pts',(-2.07763572815337,4.60025200546567,0.5598089309609));
#12745=CARTESIAN_POINT('Ctrl Pts',(-2.10450838578849,4.58997453037713,0.446901634662001));
#12746=CARTESIAN_POINT('Ctrl Pts',(-2.12237362560969,4.57969697944582,0.332700398221384));
#12747=CARTESIAN_POINT('Ctrl Pts',(-2.14719082634332,4.56542009052269,0.174059650202283));
#12748=CARTESIAN_POINT('Ctrl Pts',(-2.15469089740905,4.55114335207784,0.0125183563644346));
#12749=CARTESIAN_POINT('Ctrl Pts',(-2.14418756886859,4.5368666433287,-0.147802409798827));
#12750=CARTESIAN_POINT('Ctrl Pts',(-2.13723154232329,4.52741162488803,-0.253977847508746));
#12751=CARTESIAN_POINT('Ctrl Pts',(-2.12237988566817,4.51795661947189,-0.359616808663046));
#12752=CARTESIAN_POINT('Ctrl Pts',(-2.09944170626511,4.50850159199649,-0.463513238179406));
#12753=CARTESIAN_POINT('Ctrl Pts',(-2.09477215260164,4.50657682031299,-0.484663563344447));
#12754=CARTESIAN_POINT('Ctrl Pts',(-2.08976750615382,4.50465204771533,-0.50574165910436));
#12755=CARTESIAN_POINT('Ctrl Pts',(-2.08443318488955,4.50272727390753,-0.52673887188011));
#12756=CARTESIAN_POINT('Ctrl Pts',(-2.0528249925357,4.49132214516846,-0.651156563922029));
#12757=CARTESIAN_POINT('Ctrl Pts',(-2.00969503857243,4.47991701802016,-0.772541532210201));
#12758=CARTESIAN_POINT('Ctrl Pts',(-1.95623195885362,4.46851187550785,-0.889203652466676));
#12759=CARTESIAN_POINT('Ctrl Pts',(-1.90007420389999,4.45653188479675,-1.0117458403876));
#12760=CARTESIAN_POINT('Ctrl Pts',(-1.832515037961,4.4445518771338,-1.12907841821667));
#12761=CARTESIAN_POINT('Ctrl Pts',(-1.75487604325656,4.43257183286906,-1.23923821120557));
#12762=CARTESIAN_POINT('Ctrl Pts',(-1.74015542163619,4.43030037508824,-1.26012488853235));
#12763=CARTESIAN_POINT('Ctrl Pts',(-1.72507229226648,4.42802891599161,-1.28075366099619));
#12764=CARTESIAN_POINT('Ctrl Pts',(-1.70963547178022,4.42575745544522,-1.30111106658976));
#12765=CARTESIAN_POINT('Ctrl Pts',(-1.64425450402648,4.41613693230257,-1.38733263532844));
#12766=CARTESIAN_POINT('Ctrl Pts',(-1.57242672947706,4.40651646136546,-1.46881371158882));
#12767=CARTESIAN_POINT('Ctrl Pts',(-1.49486263555717,4.39689601833018,-1.54439705008315));
#12768=CARTESIAN_POINT('Ctrl Pts',(-1.42506126093028,4.38823840222916,-1.61241590596306));
#12769=CARTESIAN_POINT('Ctrl Pts',(-1.35061536726574,4.37958080872456,-1.67565804297037));
#12770=CARTESIAN_POINT('Ctrl Pts',(-1.27207216031375,4.37092322010378,-1.73330101803169));
#12771=CARTESIAN_POINT('Ctrl Pts',(-1.20513370597715,4.36354478951702,-1.78242724808653));
#12772=CARTESIAN_POINT('Ctrl Pts',(-1.13521995499769,4.35616636247752,-1.82748687396669));
#12773=CARTESIAN_POINT('Ctrl Pts',(-1.06291994134801,4.34878792802094,-1.86831238411785));
#12774=CARTESIAN_POINT('Ctrl Pts',(-0.965762182306972,4.33887268567387,
-1.92317426972154));
#12775=CARTESIAN_POINT('Ctrl Pts',(-0.864335597444932,4.32895737015848,
-1.97037545764872));
#12776=CARTESIAN_POINT('Ctrl Pts',(-0.759915575653579,4.31904203459314,
-2.0096134761703));
#12777=CARTESIAN_POINT('Ctrl Pts',(-0.653808176651047,4.30896647198526,
-2.04948556215451));
#12778=CARTESIAN_POINT('Ctrl Pts',(-0.544608532407727,4.29889088867419,
-2.08113553109579));
#12779=CARTESIAN_POINT('Ctrl Pts',(-0.433629444273735,4.28881534039535,
-2.10419960703838));
#12780=CARTESIAN_POINT('Ctrl Pts',(-0.371222605833282,4.28314956025416,
-2.11716922217335));
#12781=CARTESIAN_POINT('Ctrl Pts',(-0.308252733748727,4.27748379119067,
-2.12742297787052));
#12782=CARTESIAN_POINT('Ctrl Pts',(-0.244952189086059,4.27181804311557,
-2.13488900026679));
#12783=CARTESIAN_POINT('Ctrl Pts',(-0.145431729722479,4.262910412793,-2.14662700319324));
#12784=CARTESIAN_POINT('Ctrl Pts',(-0.0450219341622343,4.25400279354217,
-2.15147742757369));
#12785=CARTESIAN_POINT('Ctrl Pts',(0.0552171185010954,4.2450951771393,-2.14912756247981));
#12786=CARTESIAN_POINT('Ctrl Pts',(0.0993365333513108,4.24117456124197,
-2.1480932882108));
#12787=CARTESIAN_POINT('Ctrl Pts',(0.143422701192644,4.23725394589637,-2.1456647903115));
#12788=CARTESIAN_POINT('Ctrl Pts',(0.187384846907493,4.23333333040127,-2.14181860089706));
#12789=CARTESIAN_POINT('Ctrl Pts',(0.287266585265252,4.22442571488989,-2.13308008100634));
#12790=CARTESIAN_POINT('Ctrl Pts',(0.386507179702926,4.21551809860677,-2.11702004911881));
#12791=CARTESIAN_POINT('Ctrl Pts',(0.484109414113608,4.20661047332809,-2.09410887618576));
#12792=CARTESIAN_POINT('Ctrl Pts',(0.527068254042148,4.20268985357178,-2.08402470734937));
#12793=CARTESIAN_POINT('Ctrl Pts',(0.569709868528226,4.19876923207281,-2.07261397057064));
#12794=CARTESIAN_POINT('Ctrl Pts',(0.611950397910045,4.19484860812996,-2.05991973801053));
#12795=CARTESIAN_POINT('Ctrl Pts',(0.72031208345076,4.18479084074316,-2.02735460549466));
#12796=CARTESIAN_POINT('Ctrl Pts',(0.826122770602239,4.17473301047741,-1.986321847705));
#12797=CARTESIAN_POINT('Ctrl Pts',(0.928169509366776,4.16467517176985,-1.93743193176917));
#12798=CARTESIAN_POINT('Ctrl Pts',(1.02922438286487,4.15471509239287,-1.88901721190607));
#12799=CARTESIAN_POINT('Ctrl Pts',(1.12658932179402,4.14475500473742,-1.83289666383873));
#12800=CARTESIAN_POINT('Ctrl Pts',(1.21906484916275,4.13479496166867,-1.7696182042326));
#12801=CARTESIAN_POINT('Ctrl Pts',(1.27141877703239,4.1291562008934,-1.73379385151805));
#12802=CARTESIAN_POINT('Ctrl Pts',(1.32220509692019,4.12351745440871,-1.69567453684527));
#12803=CARTESIAN_POINT('Ctrl Pts',(1.37120083966543,4.11787873180722,-1.65535441079667));
#12804=CARTESIAN_POINT('Ctrl Pts',(1.43531317852335,4.11050030107228,-1.60259436596047));
#12805=CARTESIAN_POINT('Ctrl Pts',(1.49634026065668,4.10312187494314,-1.54607890137562));
#12806=CARTESIAN_POINT('Ctrl Pts',(1.55373108906351,4.09574344359535,-1.48607526842546));
#12807=CARTESIAN_POINT('Ctrl Pts',(1.62856052425888,4.08612302399678,-1.40783910965279));
#12808=CARTESIAN_POINT('Ctrl Pts',(1.69720621922258,4.07650259552624,-1.32367226301154));
#12809=CARTESIAN_POINT('Ctrl Pts',(1.75912692331253,4.06688213640668,-1.23481791804035));
#12810=CARTESIAN_POINT('Ctrl Pts',(1.81485044483566,4.05822451746178,-1.15485634335877));
#12811=CARTESIAN_POINT('Ctrl Pts',(1.86512796421619,4.04956687369575,-1.07109975029203));
#12812=CARTESIAN_POINT('Ctrl Pts',(1.90959783197144,4.04090918923747,-0.9844691833771));
#12813=CARTESIAN_POINT('Ctrl Pts',(1.97123887704193,4.02890850776849,-0.864387902517969));
#12814=CARTESIAN_POINT('Ctrl Pts',(2.02184616441858,4.01690787343384,-0.738562419696407));
#12815=CARTESIAN_POINT('Ctrl Pts',(2.06046390294875,4.00490726149064,-0.609168226113287));
#12816=CARTESIAN_POINT('Ctrl Pts',(2.09724139047428,3.99347851468055,-0.485940053737005));
#12817=CARTESIAN_POINT('Ctrl Pts',(2.12314494697457,3.98204978817869,-0.359473900304984));
#12818=CARTESIAN_POINT('Ctrl Pts',(2.13730195886065,3.97062106061345,-0.231649889169576));
#12819=CARTESIAN_POINT('Ctrl Pts',(2.14006086779408,3.96839383788938,-0.20673963204283));
#12820=CARTESIAN_POINT('Ctrl Pts',(2.14237351304075,3.96616661512494,-0.181777842159215));
#12821=CARTESIAN_POINT('Ctrl Pts',(2.14423320644537,3.96393939216193,-0.156778500878331));
#12822=CARTESIAN_POINT('Ctrl Pts',(2.14584035961558,3.96201461873592,-0.135173987740378));
#12823=CARTESIAN_POINT('Ctrl Pts',(2.14710880128732,3.96008984632443,-0.11354706786211));
#12824=CARTESIAN_POINT('Ctrl Pts',(2.14803469848385,3.95816507465925,-0.0919072041729757));
#12825=CARTESIAN_POINT('Ctrl Pts',(2.15490242896436,3.94388831360785,0.0686038676925654));
#12826=CARTESIAN_POINT('Ctrl Pts',(2.14292173815727,3.92961159361594,0.229824217247526));
#12827=CARTESIAN_POINT('Ctrl Pts',(2.11346589439703,3.91533480522002,0.38778518067942));
#12828=CARTESIAN_POINT('Ctrl Pts',(2.09395834183425,3.90587979852159,0.492397081193876));
#12829=CARTESIAN_POINT('Ctrl Pts',(2.06678697144009,3.89642476182156,0.595580002711112));
#12830=CARTESIAN_POINT('Ctrl Pts',(2.03235718415981,3.88696966332459,0.696192242023687));
#12831=CARTESIAN_POINT('Ctrl Pts',(1.98920577051361,3.87511943424862,0.822291201657256));
#12832=CARTESIAN_POINT('Ctrl Pts',(1.93455889875707,3.86326931194115,0.944616676195892));
#12833=CARTESIAN_POINT('Ctrl Pts',(1.86911866174675,3.85141922753818,1.06083676473496));
#12834=CARTESIAN_POINT('Ctrl Pts',(1.81236306818258,3.84114178043831,1.16163316172961));
#12835=CARTESIAN_POINT('Ctrl Pts',(1.74748992338059,3.83086436184984,1.25783628961372));
#12836=CARTESIAN_POINT('Ctrl Pts',(1.674988639014,3.82058692684825,1.34792917439058));
#12837=CARTESIAN_POINT('Ctrl Pts',(1.65009381796463,3.81705795619006,1.37886443662677));
#12838=CARTESIAN_POINT('Ctrl Pts',(1.62429984567893,3.81352898359671,1.40907937140894));
#12839=CARTESIAN_POINT('Ctrl Pts',(1.59766160651677,3.81000000724943,1.43854059611177));
#12840=CARTESIAN_POINT('Ctrl Pts',(1.51729984919832,3.79935385533692,1.5274186850673));
#12841=CARTESIAN_POINT('Ctrl Pts',(1.42935673322849,3.788707678032,1.60933109459253));
#12842=CARTESIAN_POINT('Ctrl Pts',(1.33529447087369,3.77806148606583,1.68349262622453));
#12843=CARTESIAN_POINT('Ctrl Pts',(1.23773059337837,3.76701897291787,1.76041493710537));
#12844=CARTESIAN_POINT('Ctrl Pts',(1.13358247687332,3.75597644399672,1.82899949817504));
#12845=CARTESIAN_POINT('Ctrl Pts',(1.0244378094136,3.74493391127711,1.88833689452043));
#12846=CARTESIAN_POINT('Ctrl Pts',(0.985218829988154,3.74096599535768,1.90965861532084));
#12847=CARTESIAN_POINT('Ctrl Pts',(0.945354382089341,3.73699807894779,1.92978598521962));
#12848=CARTESIAN_POINT('Ctrl Pts',(0.904917226262744,3.73303016260304,1.94867544599454));
#12849=CARTESIAN_POINT('Ctrl Pts',(0.810733708389469,3.72378835732925,1.99267151421802));
#12850=CARTESIAN_POINT('Ctrl Pts',(0.7133192154603,3.71454658877054,2.03000494321816));
#12851=CARTESIAN_POINT('Ctrl Pts',(0.613707760854252,3.70530484082039,2.06003066325302));
#12852=CARTESIAN_POINT('Ctrl Pts',(0.533591656612385,3.69787183178464,2.08417993128412));
#12853=CARTESIAN_POINT('Ctrl Pts',(0.452055362080121,3.69043883608009,2.10360258824914));
#12854=CARTESIAN_POINT('Ctrl Pts',(0.36964756560502,3.68300584532693,2.11798505125678));
#12855=CARTESIAN_POINT('Ctrl Pts',(0.270069332753102,3.67402412131944,2.13536423516435));
#12856=CARTESIAN_POINT('Ctrl Pts',(0.169219256536759,3.66504240454161,2.14538279323063));
#12857=CARTESIAN_POINT('Ctrl Pts',(0.0681960517151269,3.65606068020844,
2.1482476056522));
#12858=CARTESIAN_POINT('Ctrl Pts',(-0.0424951484675184,3.64621939821879,
2.15138658273971));
#12859=CARTESIAN_POINT('Ctrl Pts',(-0.153392117145235,3.63637803514527,
2.14594608438397));
#12860=CARTESIAN_POINT('Ctrl Pts',(-0.263251987505055,3.62653665222612,
2.13220831198733));
#12861=CARTESIAN_POINT('Ctrl Pts',(-0.374061522960836,3.61661019713436,
2.11835178573727));
#12862=CARTESIAN_POINT('Ctrl Pts',(-0.483817310267165,3.6066837218524,2.09605372877359));
#12863=CARTESIAN_POINT('Ctrl Pts',(-0.591242871291941,3.59675728922043,
2.06555172845434));
#12864=CARTESIAN_POINT('Ctrl Pts',(-0.654973047937661,3.59086843652037,
2.04745642739331));
#12865=CARTESIAN_POINT('Ctrl Pts',(-0.717882993580609,3.58497959883076,
2.0264728153448));
#12866=CARTESIAN_POINT('Ctrl Pts',(-0.779703005872109,3.57909078927208,
2.00264238198665));
#12867=CARTESIAN_POINT('Ctrl Pts',(-0.873721151897173,3.57013487133419,
1.96640018338044));
#12868=CARTESIAN_POINT('Ctrl Pts',(-0.965256992030045,3.5611789590792,1.92355258044361));
#12869=CARTESIAN_POINT('Ctrl Pts',(-1.05320797236887,3.55222304345234,1.87429990683767));
#12870=CARTESIAN_POINT('Ctrl Pts',(-1.07549803889703,3.54995327960918,1.86181743799949));
#12871=CARTESIAN_POINT('Ctrl Pts',(-1.09755792374472,3.54768351554944,1.84892381735926));
#12872=CARTESIAN_POINT('Ctrl Pts',(-1.11936987351294,3.54541375112573,1.83562280614203));
#12873=CARTESIAN_POINT('Ctrl Pts',(-1.20552346155375,3.53644855767956,1.78308601538688));
#12874=CARTESIAN_POINT('Ctrl Pts',(-1.28780634668958,3.52748335855489,1.72419020306907));
#12875=CARTESIAN_POINT('Ctrl Pts',(-1.36552068167549,3.51851814466872,1.65981285611839));
#12876=CARTESIAN_POINT('Ctrl Pts',(-1.41289880986703,3.51305255002855,1.62056555126769));
#12877=CARTESIAN_POINT('Ctrl Pts',(-1.45857956462854,3.50758694990203,1.57928181390491));
#12878=CARTESIAN_POINT('Ctrl Pts',(-1.50241189349563,3.50212134223111,1.5361667894027));
#12879=CARTESIAN_POINT('Ctrl Pts',(-1.58533092929737,3.49178187522451,1.4546047014942));
#12880=CARTESIAN_POINT('Ctrl Pts',(-1.66173246807074,3.4814423680699,1.36640237637631));
#12881=CARTESIAN_POINT('Ctrl Pts',(-1.73071604045821,3.47110286104971,1.27273692558878));
#12882=CARTESIAN_POINT('Ctrl Pts',(-1.79843625189437,3.46095271113256,1.18078685817321));
#12883=CARTESIAN_POINT('Ctrl Pts',(-1.8590084362504,3.45080256134496,1.08357076733883));
#12884=CARTESIAN_POINT('Ctrl Pts',(-1.91153970529294,3.44065244979636,0.982175567345101));
#12885=CARTESIAN_POINT('Ctrl Pts',(-1.938281193755,3.43548544934477,0.930559480009675));
#12886=CARTESIAN_POINT('Ctrl Pts',(-1.9629382272084,3.43031845880245,0.877860092613464));
#12887=CARTESIAN_POINT('Ctrl Pts',(-1.98538790967749,3.42515148319672,0.824219506712342));
#12888=CARTESIAN_POINT('Ctrl Pts',(-2.01047811662508,3.41937676957128,0.764269732237709));
#12889=CARTESIAN_POINT('Ctrl Pts',(-2.03279986241567,3.41360206091566,0.703169210488066));
#12890=CARTESIAN_POINT('Ctrl Pts',(-2.05217699413633,3.40782735126269,0.641147085472373));
#12891=CARTESIAN_POINT('Ctrl Pts',(-2.08650455004101,3.39759716491195,0.531271795646451));
#12892=CARTESIAN_POINT('Ctrl Pts',(-2.11158768355524,3.38736697543116,0.418503998794418));
#12893=CARTESIAN_POINT('Ctrl Pts',(-2.12751323101412,3.37713674964412,0.304449183630048));
#12894=CARTESIAN_POINT('Ctrl Pts',(-2.14253799199325,3.36748516952673,0.196845577487949));
#12895=CARTESIAN_POINT('Ctrl Pts',(-2.14941231931092,3.3578335570941,0.0880975860949286));
#12896=CARTESIAN_POINT('Ctrl Pts',(-2.14825154044069,3.34818188448715,-0.0204499931582646));
#12897=CARTESIAN_POINT('Ctrl Pts',(-2.14664614148736,3.33483327391323,-0.170575201834474));
#12898=CARTESIAN_POINT('Ctrl Pts',(-2.12967714969834,3.32148476313739,-0.3206566064012));
#12899=CARTESIAN_POINT('Ctrl Pts',(-2.09747674712209,3.30813627916616,-0.46737274837291));
#12900=CARTESIAN_POINT('Ctrl Pts',(-2.06778615671754,3.29582822279411,-0.602653320306828));
#12901=CARTESIAN_POINT('Ctrl Pts',(-2.0251455732522,3.283520189211,-0.735073410914382));
#12902=CARTESIAN_POINT('Ctrl Pts',(-1.96963201681683,3.27121212119573,-0.862000140862884));
#12903=CARTESIAN_POINT('Ctrl Pts',(-1.96818526952361,3.27089135875086,-0.865307997804165));
#12904=CARTESIAN_POINT('Ctrl Pts',(-1.96672984517333,3.27057059632982,-0.868611967399311));
#12905=CARTESIAN_POINT('Ctrl Pts',(-1.965265747465,3.27024983393156,-0.871912003499029));
#12906=CARTESIAN_POINT('Ctrl Pts',(-1.8996909223591,3.25588334865774,-1.01971586170543));
#12907=CARTESIAN_POINT('Ctrl Pts',(-1.81672182290529,3.24151690909339,-1.15962744970581));
#12908=CARTESIAN_POINT('Ctrl Pts',(-1.71938423090768,3.22715042128175,-1.28871874275917));
#12909=CARTESIAN_POINT('Ctrl Pts',(-1.64506358019347,3.21618110613098,-1.38728445313241));
#12910=CARTESIAN_POINT('Ctrl Pts',(-1.56236501271207,3.20521176285271,-1.47954265375796));
#12911=CARTESIAN_POINT('Ctrl Pts',(-1.47261591349647,3.19424234962399,-1.56419538135796));
#12912=CARTESIAN_POINT('Ctrl Pts',(-1.38612102881625,3.18367067658749,-1.64577868387154));
#12913=CARTESIAN_POINT('Ctrl Pts',(-1.29291648826503,3.17309908312012,-1.72044327963702));
#12914=CARTESIAN_POINT('Ctrl Pts',(-1.19420413823089,3.1625275255954,-1.7869012585407));
#12915=CARTESIAN_POINT('Ctrl Pts',(-1.10127855845529,3.15257569979269,-1.84946330086065));
#12916=CARTESIAN_POINT('Ctrl Pts',(-1.0034731816617,3.14262390584207,-1.90475212557082));
#12917=CARTESIAN_POINT('Ctrl Pts',(-0.901821977267037,3.13267210734858,
-1.95172157886228));
#12918=CARTESIAN_POINT('Ctrl Pts',(-0.849390496460778,3.1275389902861,-1.97594832564208));
#12919=CARTESIAN_POINT('Ctrl Pts',(-0.79593626755812,3.122405872015,-1.99796226104316));
#12920=CARTESIAN_POINT('Ctrl Pts',(-0.741660178022841,3.11727274754091,
-2.01774690915893));
#12921=CARTESIAN_POINT('Ctrl Pts',(-0.633624534486916,3.10705534959171,
-2.05712791854301));
#12922=CARTESIAN_POINT('Ctrl Pts',(-0.522430016986537,3.09683790245466,
-2.08764666535729));
#12923=CARTESIAN_POINT('Ctrl Pts',(-0.409527264222796,3.08662043823546,
-2.10925869119181));
#12924=CARTESIAN_POINT('Ctrl Pts',(-0.293519898919739,3.07612201304093,
-2.13146500693302));
#12925=CARTESIAN_POINT('Ctrl Pts',(-0.175707713868161,3.06562356981184,
-2.1442683506305));
#12926=CARTESIAN_POINT('Ctrl Pts',(-0.0576437673723606,3.05512514337599,
-2.14757037715293));
#12927=CARTESIAN_POINT('Ctrl Pts',(-0.00208063382617425,3.05018438468214,
-2.14912437349207));
#12928=CARTESIAN_POINT('Ctrl Pts',(0.0535384230342057,3.04524362970769,
-2.1485732579766));
#12929=CARTESIAN_POINT('Ctrl Pts',(0.109051688665274,3.04030288208286,-2.14590278660309));
#12930=CARTESIAN_POINT('Ctrl Pts',(0.210388807281865,3.03128375625016,-2.14102795405156));
#12931=CARTESIAN_POINT('Ctrl Pts',(0.311481707292144,3.02226465441966,-2.12908060919421));
#12932=CARTESIAN_POINT('Ctrl Pts',(0.411193133653393,3.013245565563,-2.10995375633487));
#12933=CARTESIAN_POINT('Ctrl Pts',(0.478110136128969,3.00719279494911,-2.09711759796421));
#12934=CARTESIAN_POINT('Ctrl Pts',(0.544404650338317,3.00114003017844,-2.08104895318567));
#12935=CARTESIAN_POINT('Ctrl Pts',(0.609733450344373,2.99508726791757,-2.06172867262875));
#12936=CARTESIAN_POINT('Ctrl Pts',(0.706933970211559,2.98608156693525,-2.03298267830558));
#12937=CARTESIAN_POINT('Ctrl Pts',(0.801995196015169,2.97707587150898,-1.99703639806845));
#12938=CARTESIAN_POINT('Ctrl Pts',(0.894009539879667,2.96807017065937,-1.95457232965125));
#12939=CARTESIAN_POINT('Ctrl Pts',(0.910141835246869,2.96649125785085,-1.94712737199109));
#12940=CARTESIAN_POINT('Ctrl Pts',(0.926180537486656,2.96491234487564,-1.93948218095153));
#12941=CARTESIAN_POINT('Ctrl Pts',(0.942120844041218,2.96333343167455,-1.93164057257274));
#12942=CARTESIAN_POINT('Ctrl Pts',(1.04169895621625,2.95347005826233,-1.88265452854005));
#12943=CARTESIAN_POINT('Ctrl Pts',(1.13747236916903,2.94360660484181,-1.82599127228637));
#12944=CARTESIAN_POINT('Ctrl Pts',(1.22844424331902,2.93374313446163,-1.76245278614713));
#12945=CARTESIAN_POINT('Ctrl Pts',(1.31952357108006,2.92386801360685,-1.69883925000107));
#12946=CARTESIAN_POINT('Ctrl Pts',(1.40579110765157,2.91399287575234,-1.62833341128625));
#12947=CARTESIAN_POINT('Ctrl Pts',(1.48621992686302,2.90411778417053,-1.55169643628954));
#12948=CARTESIAN_POINT('Ctrl Pts',(1.53442058880381,2.898199682231,-1.50576821105636));
#12949=CARTESIAN_POINT('Ctrl Pts',(1.58052365801219,2.89228159691056,-1.45763717410918));
#12950=CARTESIAN_POINT('Ctrl Pts',(1.62430103503315,2.88636354182797,-1.40746151925886));
#12951=CARTESIAN_POINT('Ctrl Pts',(1.69173498938177,2.87724746673555,-1.3301717625663));
#12952=CARTESIAN_POINT('Ctrl Pts',(1.75365442585972,2.8681313954874,-1.24801752262837));
#12953=CARTESIAN_POINT('Ctrl Pts',(1.80912283730287,2.85901531580153,-1.16170605324713));
#12954=CARTESIAN_POINT('Ctrl Pts',(1.81220681460461,2.85850847267946,-1.1569072388314));
#12955=CARTESIAN_POINT('Ctrl Pts',(1.81527086018526,2.85800162953131,-1.15209558261765));
#12956=CARTESIAN_POINT('Ctrl Pts',(1.81831481673788,2.85749478635496,-1.14727120926561));
#12957=CARTESIAN_POINT('Ctrl Pts',(1.87318565161585,2.84835835232332,-1.0603063038826));
#12958=CARTESIAN_POINT('Ctrl Pts',(1.92152469700568,2.83922190913028,-0.96920711629221));
#12959=CARTESIAN_POINT('Ctrl Pts',(1.96308343251013,2.83008544441134,-0.87512601001788));
#12960=CARTESIAN_POINT('Ctrl Pts',(1.9944561004723,2.82318833191511,-0.804104231495727));
#12961=CARTESIAN_POINT('Ctrl Pts',(2.02196578264352,2.81629120715186,-0.731383902142148));
#12962=CARTESIAN_POINT('Ctrl Pts',(2.04552456127386,2.80939406480244,-0.657465805531989));
#12963=CARTESIAN_POINT('Ctrl Pts',(2.08241088493445,2.79859510832741,-0.541731162462456));
#12964=CARTESIAN_POINT('Ctrl Pts',(2.10967171517931,2.78779614223852,-0.422897417519029));
#12965=CARTESIAN_POINT('Ctrl Pts',(2.12696593385866,2.77699718589282,-0.302632173723326));
#12966=CARTESIAN_POINT('Ctrl Pts',(2.14377041553965,2.76650403396443,-0.185772596329485));
#12967=CARTESIAN_POINT('Ctrl Pts',(2.15116481342204,2.75601089123524,-0.0675600796035336));
#12968=CARTESIAN_POINT('Ctrl Pts',(2.14878813127568,2.74551777546388,0.0504759594829834));
#12969=CARTESIAN_POINT('Ctrl Pts',(2.14779957088035,2.74115325465865,0.0995720296670876));
#12970=CARTESIAN_POINT('Ctrl Pts',(2.14511995457142,2.73678873851731,0.148637459180571));
#12971=CARTESIAN_POINT('Ctrl Pts',(2.14072071578196,2.73242422831781,0.19756138083896));
#12972=CARTESIAN_POINT('Ctrl Pts',(2.13651687479091,2.72825357340213,0.244312284155051));
#12973=CARTESIAN_POINT('Ctrl Pts',(2.13074439087573,2.72408292230982,0.290913680125547));
#12974=CARTESIAN_POINT('Ctrl Pts',(2.12338297676972,2.71991227241574,0.337260632528063));
#12975=CARTESIAN_POINT('Ctrl Pts',(2.10352655248463,2.70866250536706,0.462275301988544));
#12976=CARTESIAN_POINT('Ctrl Pts',(2.0721060016905,2.69741274703639,0.585437161112324));
#12977=CARTESIAN_POINT('Ctrl Pts',(2.03016918451094,2.68616294590418,0.704921112297282));
#12978=CARTESIAN_POINT('Ctrl Pts',(1.99201131259478,2.67592686935963,0.81363831145501));
#12979=CARTESIAN_POINT('Ctrl Pts',(1.94514810499035,2.66569075737976,0.919309952190526));
#12980=CARTESIAN_POINT('Ctrl Pts',(1.89039889086094,2.65545457115502,1.0205837859347));
#12981=CARTESIAN_POINT('Ctrl Pts',(1.80901360106348,2.64023837133247,1.17112841820445));
#12982=CARTESIAN_POINT('Ctrl Pts',(1.70998760896235,2.62502233564322,1.31236306612878));
#12983=CARTESIAN_POINT('Ctrl Pts',(1.59571189358983,2.60980632287908,1.43987397263786));
#12984=CARTESIAN_POINT('Ctrl Pts',(1.52693807041457,2.6006489671989,1.51661304627731));
#12985=CARTESIAN_POINT('Ctrl Pts',(1.45264173282485,2.591491619822,1.5883807320115));
#12986=CARTESIAN_POINT('Ctrl Pts',(1.3733508076554,2.58233424996849,1.6542090433471));
#12987=CARTESIAN_POINT('Ctrl Pts',(1.36224054081993,2.58105111671754,1.66343292492881));
#12988=CARTESIAN_POINT('Ctrl Pts',(1.35103221931852,2.57976798302529,1.6725401883537));
#12989=CARTESIAN_POINT('Ctrl Pts',(1.33972865760694,2.57848484880706,1.68152979797504));
#12990=CARTESIAN_POINT('Ctrl Pts',(1.23494836182595,2.56659061702923,1.76486051966376));
#12991=CARTESIAN_POINT('Ctrl Pts',(1.122164294256,2.55469639933387,1.83794380682689));
#12992=CARTESIAN_POINT('Ctrl Pts',(1.00362766456432,2.54280216347611,1.90008356090546));
#12993=CARTESIAN_POINT('Ctrl Pts',(0.878254391920993,2.53022192326716,1.96580724775522));
#12994=CARTESIAN_POINT('Ctrl Pts',(0.746444791840392,2.51764166274032,2.01928946994072));
#12995=CARTESIAN_POINT('Ctrl Pts',(0.610817914220216,2.50506134374346,2.05967163702932));
#12996=CARTESIAN_POINT('Ctrl Pts',(0.598073850852332,2.50387924484612,2.06346611276554));
#12997=CARTESIAN_POINT('Ctrl Pts',(0.585296060455977,2.50269714543254,2.06714489505422));
#12998=CARTESIAN_POINT('Ctrl Pts',(0.572486702820834,2.50151504547105,2.07070725264017));
#12999=CARTESIAN_POINT('Ctrl Pts',(0.465857401602194,2.49167485703586,2.10036148752846));
#13000=CARTESIAN_POINT('Ctrl Pts',(0.356869727964285,2.48183472835482,2.12199121968651));
#13001=CARTESIAN_POINT('Ctrl Pts',(0.246875167750652,2.47199463026813,2.13508829993763));
#13002=CARTESIAN_POINT('Ctrl Pts',(0.145383698683764,2.46291521753498,2.14717291496397));
#13003=CARTESIAN_POINT('Ctrl Pts',(0.04303616977167,2.45383583084887,2.15199328339809));
#13004=CARTESIAN_POINT('Ctrl Pts',(-0.0590937688555852,2.44475644730326,
2.14918773647839));
#13005=CARTESIAN_POINT('Ctrl Pts',(-0.134875091103585,2.43801946400991,
2.14710599572674));
#13006=CARTESIAN_POINT('Ctrl Pts',(-0.2105363151451,2.43128248244564,2.14082641582439));
#13007=CARTESIAN_POINT('Ctrl Pts',(-0.285647338284483,2.42454549325238,
2.13052149366505));
#13008=CARTESIAN_POINT('Ctrl Pts',(-0.396965761014252,2.41456092667886,
2.11524906582178));
#13009=CARTESIAN_POINT('Ctrl Pts',(-0.507018890481444,2.40457629337122,
2.09114945184087));
#13010=CARTESIAN_POINT('Ctrl Pts',(-0.6145848234177,2.39459164121287,2.05877934147919));
#13011=CARTESIAN_POINT('Ctrl Pts',(-0.724190762137535,2.38441762846799,
2.02579532659821));
#13012=CARTESIAN_POINT('Ctrl Pts',(-0.831215595269355,2.37424359615059,
1.98422376310785));
#13013=CARTESIAN_POINT('Ctrl Pts',(-0.934359320682798,2.3640695949205,1.93460088691591));
#13014=CARTESIAN_POINT('Ctrl Pts',(-0.990097929254591,2.35857159036521,
1.90778481001756));
#13015=CARTESIAN_POINT('Ctrl Pts',(-1.04470289635645,2.35307359488832,1.87861664475033));
#13016=CARTESIAN_POINT('Ctrl Pts',(-1.09796608325633,2.34757561648456,1.84717540290619));
#13017=CARTESIAN_POINT('Ctrl Pts',(-1.18421742323335,2.33867250662407,1.79626126506656));
#13018=CARTESIAN_POINT('Ctrl Pts',(-1.26701772081672,2.32976941108325,1.73934057733943));
#13019=CARTESIAN_POINT('Ctrl Pts',(-1.34533819526139,2.32086632059572,1.67681359440466));
#13020=CARTESIAN_POINT('Ctrl Pts',(-1.38550722784109,2.31630010040375,1.64474473332553));
#13021=CARTESIAN_POINT('Ctrl Pts',(-1.42449815487176,2.31173388154103,1.61120193998494));
#13022=CARTESIAN_POINT('Ctrl Pts',(-1.46217489296344,2.30716766275741,1.57624382072239));
#13023=CARTESIAN_POINT('Ctrl Pts',(-1.53563328275405,2.29826489950704,1.50808592592571));
#13024=CARTESIAN_POINT('Ctrl Pts',(-1.60409331664952,2.28936213655732,1.43454604043423));
#13025=CARTESIAN_POINT('Ctrl Pts',(-1.66706033649241,2.28045936464286,1.35660998984868));
#13026=CARTESIAN_POINT('Ctrl Pts',(-1.69029001396386,2.27717497035691,1.32785796501062));
#13027=CARTESIAN_POINT('Ctrl Pts',(-1.71277250270999,2.27389057485086,1.29850792734728));
#13028=CARTESIAN_POINT('Ctrl Pts',(-1.73448450182989,2.27060617765949,1.26861028057278));
#13029=CARTESIAN_POINT('Ctrl Pts',(-1.79972704223425,2.26073686920573,1.17877062937763));
#13030=CARTESIAN_POINT('Ctrl Pts',(-1.85806026613614,2.25086748884915,1.08392925964598));
#13031=CARTESIAN_POINT('Ctrl Pts',(-1.90894278137274,2.2409980982588,0.985246190110895));
#13032=CARTESIAN_POINT('Ctrl Pts',(-1.95948299046544,2.23119510283425,0.887226999333456));
#13033=CARTESIAN_POINT('Ctrl Pts',(-2.00267295250023,2.22139209731318,0.785416381034645));
#13034=CARTESIAN_POINT('Ctrl Pts',(-2.03793790884311,2.21158914212838,0.680927388260187));
#13035=CARTESIAN_POINT('Ctrl Pts',(-2.05946575212243,2.20560483065381,0.617141043567426));
#13036=CARTESIAN_POINT('Ctrl Pts',(-2.07803935625401,2.19962053793762,0.552356188959628));
#13037=CARTESIAN_POINT('Ctrl Pts',(-2.09351843408538,2.19363627772794,0.486824635297257));
#13038=CARTESIAN_POINT('Ctrl Pts',(-2.11426298230575,2.1856163700929,0.399001414191062));
#13039=CARTESIAN_POINT('Ctrl Pts',(-2.12944394678572,2.17759645972531,0.309845908133398));
#13040=CARTESIAN_POINT('Ctrl Pts',(-2.13870728451891,2.16957654356607,0.22007078798899));
#13041=CARTESIAN_POINT('Ctrl Pts',(-2.1494919731514,2.16023948805461,0.115551580594407));
#13042=CARTESIAN_POINT('Ctrl Pts',(-2.15225428035161,2.15090242469288,0.0101933317018818));
#13043=CARTESIAN_POINT('Ctrl Pts',(-2.14728720710796,2.14156534865332,-0.0948041580853045));
#13044=CARTESIAN_POINT('Ctrl Pts',(-2.14287211193829,2.13326587785856,-0.188133546891817));
#13045=CARTESIAN_POINT('Ctrl Pts',(-2.13235100881986,2.12496639704717,-0.28117718946733));
#13046=CARTESIAN_POINT('Ctrl Pts',(-2.1159636378089,2.11666690282892,-0.373098825557915));
#13047=CARTESIAN_POINT('Ctrl Pts',(2.551614418722,6.316751913189,-1.211595605458));
#13048=CARTESIAN_POINT('Ctrl Pts',(2.842552710281,6.270890802077,-0.598880986523));
#13049=CARTESIAN_POINT('Ctrl Pts',(2.962035735699,6.179168579855,0.8419695182761));
#13050=CARTESIAN_POINT('Ctrl Pts',(1.670619315018,6.041585246522,2.587364402054));
#13051=CARTESIAN_POINT('Ctrl Pts',(-0.4512378705897,5.904001913189,3.046441196415));
#13052=CARTESIAN_POINT('Ctrl Pts',(-2.348791901428,5.766418579855,1.991932600627));
#13053=CARTESIAN_POINT('Ctrl Pts',(-3.079263577893,5.628835246522,-0.05240707813364));
#13054=CARTESIAN_POINT('Ctrl Pts',(-2.279655662895,5.491251913189,-2.07069305665));
#13055=CARTESIAN_POINT('Ctrl Pts',(-0.3472977925631,5.353668579855,-3.060063551872));
#13056=CARTESIAN_POINT('Ctrl Pts',(1.757631370145,5.216085246522,-2.528900044009));
#13057=CARTESIAN_POINT('Ctrl Pts',(2.989200566047,5.078501913189,-0.7411366794348));
#13058=CARTESIAN_POINT('Ctrl Pts',(2.735448240199,4.940918579855,1.414894540471));
#13059=CARTESIAN_POINT('Ctrl Pts',(1.122462847131,4.803335246522,2.86787042401));
#13060=CARTESIAN_POINT('Ctrl Pts',(-1.048269748206,4.665751913189,2.895813211186));
#13061=CARTESIAN_POINT('Ctrl Pts',(-2.698121387469,4.528168579855,1.484838239147));
#13062=CARTESIAN_POINT('Ctrl Pts',(-3.007287528446,4.390585246522,-0.6639467894038));
#13063=CARTESIAN_POINT('Ctrl Pts',(-1.822144778546,4.253001913189,-2.482819369995));
#13064=CARTESIAN_POINT('Ctrl Pts',(0.2684142700615,4.115418579855,-3.067989145611));
#13065=CARTESIAN_POINT('Ctrl Pts',(2.225599364098,3.977835246522,-2.12868764466));
#13066=CARTESIAN_POINT('Ctrl Pts',(3.076893223598,3.840251913189,-0.1316499467573));
#13067=CARTESIAN_POINT('Ctrl Pts',(2.399291406589,3.702668579855,1.930804071939));
#13068=CARTESIAN_POINT('Ctrl Pts',(0.5294914882953,3.565085246522,3.03384943313));
#13069=CARTESIAN_POINT('Ctrl Pts',(-1.603410587237,3.427501913189,2.629387400296));
#13070=CARTESIAN_POINT('Ctrl Pts',(-2.939584493455,3.289918579855,0.9183935111373));
#13071=CARTESIAN_POINT('Ctrl Pts',(-2.815090858966,3.152335246522,-1.248946378924));
#13072=CARTESIAN_POINT('Ctrl Pts',(-1.291790116112,3.014751913189,-2.795689854368));
#13073=CARTESIAN_POINT('Ctrl Pts',(0.8733960180478,2.877168579855,-2.953266681808));
#13074=CARTESIAN_POINT('Ctrl Pts',(2.604594646812,2.739585246522,-1.643376524728));
#13075=CARTESIAN_POINT('Ctrl Pts',(3.041583038692,2.602001913189,0.4830976119985));
#13076=CARTESIAN_POINT('Ctrl Pts',(1.967213008604,2.464418579855,2.369534101977));
#13077=CARTESIAN_POINT('Ctrl Pts',(-0.08462640871746,2.326835246522,3.078515543247));
#13078=CARTESIAN_POINT('Ctrl Pts',(-2.094529967139,2.189251913189,2.257956523383));
#13079=CARTESIAN_POINT('Ctrl Pts',(-3.063242229715,2.051668579855,0.3148260017099));
#13080=CARTESIAN_POINT('Ctrl Pts',(-2.695373355482,1.959946357633,-1.083386736722));
#13081=CARTESIAN_POINT('Ctrl Pts',(-2.302458293298,1.914085246522,-1.63627193969));
#13082=CARTESIAN_POINT('Ctrl Pts',(2.566245858361,6.354663466539,-1.218543123796));
#13083=CARTESIAN_POINT('Ctrl Pts',(2.858852445106,6.308802355428,-0.6023150833602));
#13084=CARTESIAN_POINT('Ctrl Pts',(2.979020608788,6.217080133205,0.8467975307274));
#13085=CARTESIAN_POINT('Ctrl Pts',(1.680198962119,6.079496799872,2.602200838859));
#13086=CARTESIAN_POINT('Ctrl Pts',(-0.4538253538779,5.941913466539,3.063910066379));
#13087=CARTESIAN_POINT('Ctrl Pts',(-2.362260318395,5.804330133205,2.003354718874));
#13088=CARTESIAN_POINT('Ctrl Pts',(-3.0969206576,5.666746799872,-0.05270759023089));
#13089=CARTESIAN_POINT('Ctrl Pts',(-2.292727639595,5.529163466539,-2.082566802247));
#13090=CARTESIAN_POINT('Ctrl Pts',(-0.3492892637867,5.391580133205,-3.077610534999));
#13091=CARTESIAN_POINT('Ctrl Pts',(1.767709960825,5.253996799872,-2.543401235127));
#13092=CARTESIAN_POINT('Ctrl Pts',(3.006341207411,5.116413466539,-0.7453864973187));
#13093=CARTESIAN_POINT('Ctrl Pts',(2.751133817737,4.978830133205,1.423007813351));
#13094=CARTESIAN_POINT('Ctrl Pts',(1.128899261377,4.841246799872,2.884315335393));
#13095=CARTESIAN_POINT('Ctrl Pts',(-1.054280725191,4.703663466539,2.912418351796));
#13096=CARTESIAN_POINT('Ctrl Pts',(-2.713592925774,4.566080133205,1.493352582423));
#13097=CARTESIAN_POINT('Ctrl Pts',(-3.024531883873,4.428496799872,-0.66775398586));
#13098=CARTESIAN_POINT('Ctrl Pts',(-1.832593301311,4.290913466539,-2.497056325814));
#13099=CARTESIAN_POINT('Ctrl Pts',(0.2699534082486,4.153330133205,-3.085581575591));
#13100=CARTESIAN_POINT('Ctrl Pts',(2.238361371758,4.015746799872,-2.140893942192));
#13101=CARTESIAN_POINT('Ctrl Pts',(3.094536711245,3.878163466539,-0.1324048524497));
#13102=CARTESIAN_POINT('Ctrl Pts',(2.413049397269,3.740580133205,1.941875667641));
#13103=CARTESIAN_POINT('Ctrl Pts',(0.5325276926267,3.602996799872,3.051246099542));
#13104=CARTESIAN_POINT('Ctrl Pts',(-1.612604846782,3.465413466539,2.64446480492));
#13105=CARTESIAN_POINT('Ctrl Pts',(-2.956440626875,3.327830133205,0.923659753217));
#13106=CARTESIAN_POINT('Ctrl Pts',(-2.831233122342,3.190246799872,-1.256108073662));
#13107=CARTESIAN_POINT('Ctrl Pts',(-1.299197484941,3.052663466539,-2.811720868715));
#13108=CARTESIAN_POINT('Ctrl Pts',(0.8784042359921,2.915080133205,-2.970201271484));
#13109=CARTESIAN_POINT('Ctrl Pts',(2.619529885098,2.777496799872,-1.652799956517));
#13110=CARTESIAN_POINT('Ctrl Pts',(3.059024051061,2.639913466539,0.4858677850693));
#13111=CARTESIAN_POINT('Ctrl Pts',(1.978493380035,2.502330133205,2.383121458644));
#13112=CARTESIAN_POINT('Ctrl Pts',(-0.08511167254962,2.364746799872,3.096168333582));
#13113=CARTESIAN_POINT('Ctrl Pts',(-2.106540398089,2.227163466539,2.270904073113));
#13114=CARTESIAN_POINT('Ctrl Pts',(-3.080807439981,2.089580133205,0.3166312735437));
#13115=CARTESIAN_POINT('Ctrl Pts',(-2.710829136052,1.997857910983,-1.089599081161));
#13116=CARTESIAN_POINT('Ctrl Pts',(-2.315661024593,1.951996799872,-1.645654632444));
#13117=CARTESIAN_POINT('Ctrl Pts',(2.610640441769,6.569665066603,-1.239623221859));
#13118=CARTESIAN_POINT('Ctrl Pts',(2.908308954861,6.523803955492,-0.6127347892973));
#13119=CARTESIAN_POINT('Ctrl Pts',(3.030555958942,6.432081733269,0.8614466429648));
#13120=CARTESIAN_POINT('Ctrl Pts',(1.709265441748,6.294498399936,2.647217422835));
#13121=CARTESIAN_POINT('Ctrl Pts',(-0.4616762725496,6.156915066603,3.116913955525));
#13122=CARTESIAN_POINT('Ctrl Pts',(-2.403126068804,6.019331733269,2.038011607992));
#13123=CARTESIAN_POINT('Ctrl Pts',(-3.150495611065,5.881748399936,-0.05361940135107));
#13124=CARTESIAN_POINT('Ctrl Pts',(-2.332390514489,5.744165066603,-2.118594015035));
#13125=CARTESIAN_POINT('Ctrl Pts',(-0.3553317679779,5.606581733269,-3.130851434404));
#13126=CARTESIAN_POINT('Ctrl Pts',(1.798290330606,5.468998399936,-2.587400619639));
#13127=CARTESIAN_POINT('Ctrl Pts',(3.058349188273,5.331415066603,-0.7582812567662));
#13128=CARTESIAN_POINT('Ctrl Pts',(2.798726856939,5.193831733269,1.447625033425));
#13129=CARTESIAN_POINT('Ctrl Pts',(1.148428571967,5.056248399936,2.934212338565));
#13130=CARTESIAN_POINT('Ctrl Pts',(-1.072519177847,4.918665066603,2.962801521053));
#13131=CARTESIAN_POINT('Ctrl Pts',(-2.760536529048,4.781081733269,1.519186726709));
#13132=CARTESIAN_POINT('Ctrl Pts',(-3.076854553017,4.643498399936,-0.679305747327));
#13133=CARTESIAN_POINT('Ctrl Pts',(-1.864296115717,4.505915066603,-2.540253969941));
#13134=CARTESIAN_POINT('Ctrl Pts',(0.2746234475825,4.368331733269,-3.138960369433));
#13135=CARTESIAN_POINT('Ctrl Pts',(2.27708374136,4.230748399936,-2.177930181092));
#13136=CARTESIAN_POINT('Ctrl Pts',(3.148070423804,4.093165066603,-0.1346953805558));
#13137=CARTESIAN_POINT('Ctrl Pts',(2.454793769651,3.955581733269,1.975469004389));
#13138=CARTESIAN_POINT('Ctrl Pts',(0.5417401166782,3.817998399936,3.104030909316));
#13139=CARTESIAN_POINT('Ctrl Pts',(-1.640501986934,3.680415066603,2.6902125313));
#13140=CARTESIAN_POINT('Ctrl Pts',(-3.007585356276,3.542831733269,0.9396385378769));
#13141=CARTESIAN_POINT('Ctrl Pts',(-2.880211833633,3.405248399936,-1.27783802384));
#13142=CARTESIAN_POINT('Ctrl Pts',(-1.321672857253,3.267665066603,-2.860362029195));
#13143=CARTESIAN_POINT('Ctrl Pts',(0.8936001261264,3.130081733269,-3.021584052154));
#13144=CARTESIAN_POINT('Ctrl Pts',(2.664846251648,2.992498399936,-1.681392449043));
#13145=CARTESIAN_POINT('Ctrl Pts',(3.11194341494,2.854915066603,0.4942730194467));
#13146=CARTESIAN_POINT('Ctrl Pts',(2.012720182232,2.717331733269,2.424348094831));
#13147=CARTESIAN_POINT('Ctrl Pts',(-0.08658405573291,2.579748399936,3.149730272273));
#13148=CARTESIAN_POINT('Ctrl Pts',(-2.142982340353,2.442165066603,2.310189412808));
#13149=CARTESIAN_POINT('Ctrl Pts',(-3.134103644012,2.304581733269,0.3221088132102));
#13150=CARTESIAN_POINT('Ctrl Pts',(-2.757724927347,2.212859511047,-1.108448521144));
#13151=CARTESIAN_POINT('Ctrl Pts',(-2.355720633912,2.166998399936,-1.674123514957));
#13152=CARTESIAN_POINT('Ctrl Pts',(2.258338232158,6.959666666667,-1.072337833508));
#13153=CARTESIAN_POINT('Ctrl Pts',(2.51583680334,6.913805555556,-0.5300471021225));
#13154=CARTESIAN_POINT('Ctrl Pts',(2.621586748321,6.822083333333,0.7451956453465));
#13155=CARTESIAN_POINT('Ctrl Pts',(1.478602504675,6.6845,2.289979201721));
#13156=CARTESIAN_POINT('Ctrl Pts',(-0.3993737170763,6.546916666667,2.696290856254));
#13157=CARTESIAN_POINT('Ctrl Pts',(-2.078827628288,6.409333333333,1.762984843976));
#13158=CARTESIAN_POINT('Ctrl Pts',(-2.725340715205,6.27175,-0.04638353950209));
#13159=CARTESIAN_POINT('Ctrl Pts',(-2.017637736288,6.134166666667,-1.832692769952));
#13160=CARTESIAN_POINT('Ctrl Pts',(-0.3073802519435,5.996583333333,-2.708347492208));
#13161=CARTESIAN_POINT('Ctrl Pts',(1.555613611568,5.859,-2.238234590927));
#13162=CARTESIAN_POINT('Ctrl Pts',(2.645629320936,5.721416666667,-0.6559522810899));
#13163=CARTESIAN_POINT('Ctrl Pts',(2.421042653468,5.583833333333,1.252270096834));
#13164=CARTESIAN_POINT('Ctrl Pts',(0.9934497717423,5.44625,2.538244562304));
#13165=CARTESIAN_POINT('Ctrl Pts',(-0.9277842422502,5.308666666667,2.562975675332));
#13166=CARTESIAN_POINT('Ctrl Pts',(-2.388006055937,5.171083333333,1.314174641526));
#13167=CARTESIAN_POINT('Ctrl Pts',(-2.661637413063,5.0335,-0.5876344041747));
#13168=CARTESIAN_POINT('Ctrl Pts',(-1.612712009983,4.895916666667,-2.19745031446));
#13169=CARTESIAN_POINT('Ctrl Pts',(0.2375634044427,4.758333333333,-2.715362138003));
#13170=CARTESIAN_POINT('Ctrl Pts',(1.969794533427,4.62075,-1.884021604905));
#13171=CARTESIAN_POINT('Ctrl Pts',(2.723242803511,4.483166666667,-0.1165184307794));
#13172=CARTESIAN_POINT('Ctrl Pts',(2.12352284649,4.345583333333,1.708882275658));
#13173=CARTESIAN_POINT('Ctrl Pts',(0.4686330594646,4.208,2.685146358783));
#13174=CARTESIAN_POINT('Ctrl Pts',(-1.419118580157,4.070416666667,2.327172181531));
#13175=CARTESIAN_POINT('Ctrl Pts',(-2.601715995771,3.932833333333,0.812835655399));
#13176=CARTESIAN_POINT('Ctrl Pts',(-2.491531348606,3.79525,-1.105395602386));
#13177=CARTESIAN_POINT('Ctrl Pts',(-1.143314987458,3.657666666667,-2.474360247008));
#13178=CARTESIAN_POINT('Ctrl Pts',(0.7730100617475,3.520083333333,-2.613825587577));
#13179=CARTESIAN_POINT('Ctrl Pts',(2.305229045192,3.3825,-1.45449093264));
#13180=CARTESIAN_POINT('Ctrl Pts',(2.691991083042,3.244916666667,0.4275715794031));
#13181=CARTESIAN_POINT('Ctrl Pts',(1.741106460104,3.107333333333,2.097185772127));
#13182=CARTESIAN_POINT('Ctrl Pts',(-0.07489966072249,2.96975,2.724678657793));
#13183=CARTESIAN_POINT('Ctrl Pts',(-1.853789925502,2.832166666667,1.998432641661));
#13184=CARTESIAN_POINT('Ctrl Pts',(-2.711160820761,2.694583333333,0.2786406876064));
#13185=CARTESIAN_POINT('Ctrl Pts',(-2.385573875881,2.602861111111,-0.9588649718392));
#13186=CARTESIAN_POINT('Ctrl Pts',(-2.037819489321,2.557,-1.448202930857));
#13187=CARTESIAN_POINT('Ctrl Pts',(1.906036022547,6.569665066603,-0.905052445157));
#13188=CARTESIAN_POINT('Ctrl Pts',(2.123364651819,6.523803955492,-0.4473594149477));
#13189=CARTESIAN_POINT('Ctrl Pts',(2.212617537701,6.432081733269,0.6289446477281));
#13190=CARTESIAN_POINT('Ctrl Pts',(1.247939567603,6.294498399936,1.932740980607));
#13191=CARTESIAN_POINT('Ctrl Pts',(-0.337071161603,6.156915066603,2.275667756983));
#13192=CARTESIAN_POINT('Ctrl Pts',(-1.754529187773,6.019331733269,1.487958079961));
#13193=CARTESIAN_POINT('Ctrl Pts',(-2.300185819346,5.881748399936,-0.03914767765311));
#13194=CARTESIAN_POINT('Ctrl Pts',(-1.702884958088,5.744165066603,-1.54679152487));
#13195=CARTESIAN_POINT('Ctrl Pts',(-0.2594287359091,5.606581733269,-2.285843550012));
#13196=CARTESIAN_POINT('Ctrl Pts',(1.312936892531,5.468998399936,-1.889068562215));
#13197=CARTESIAN_POINT('Ctrl Pts',(2.2329094536,5.331415066603,-0.5536233054136));
#13198=CARTESIAN_POINT('Ctrl Pts',(2.043358449998,5.193831733269,1.056915160243));
#13199=CARTESIAN_POINT('Ctrl Pts',(0.8384709715172,5.056248399936,2.142276786043));
#13200=CARTESIAN_POINT('Ctrl Pts',(-0.7830493066535,4.918665066603,2.16314982961));
#13201=CARTESIAN_POINT('Ctrl Pts',(-2.015475582826,4.781081733269,1.109162556342));
#13202=CARTESIAN_POINT('Ctrl Pts',(-2.246420273109,4.643498399936,-0.4959630610224));
#13203=CARTESIAN_POINT('Ctrl Pts',(-1.361127904248,4.505915066603,-1.85464665898));
#13204=CARTESIAN_POINT('Ctrl Pts',(0.200503361303,4.368331733269,-2.291763906573));
#13205=CARTESIAN_POINT('Ctrl Pts',(1.662505325493,4.230748399936,-1.590113028717));
#13206=CARTESIAN_POINT('Ctrl Pts',(2.298415183218,4.093165066603,-0.09834148100305));
#13207=CARTESIAN_POINT('Ctrl Pts',(1.792251923328,3.955581733269,1.442295546927));
#13208=CARTESIAN_POINT('Ctrl Pts',(0.395526002251,3.817998399936,2.266261808251));
#13209=CARTESIAN_POINT('Ctrl Pts',(-1.19773517338,3.680415066603,1.964131831763));
#13210=CARTESIAN_POINT('Ctrl Pts',(-2.195846635266,3.542831733269,0.6860327729212));
#13211=CARTESIAN_POINT('Ctrl Pts',(-2.10285086358,3.405248399936,-0.9329531809324));
#13212=CARTESIAN_POINT('Ctrl Pts',(-0.964957117664,3.267665066603,-2.088358464821));
#13213=CARTESIAN_POINT('Ctrl Pts',(0.6524199973687,3.130081733269,-2.206067123));
#13214=CARTESIAN_POINT('Ctrl Pts',(1.945611838737,2.992498399936,-1.227589416237));
#13215=CARTESIAN_POINT('Ctrl Pts',(2.272038751145,2.854915066603,0.3608701393595));
#13216=CARTESIAN_POINT('Ctrl Pts',(1.469492737975,2.717331733269,1.770023449422));
#13217=CARTESIAN_POINT('Ctrl Pts',(-0.06321526571209,2.579748399936,2.299627043313));
#13218=CARTESIAN_POINT('Ctrl Pts',(-1.56459751065,2.442165066603,1.686675870514));
#13219=CARTESIAN_POINT('Ctrl Pts',(-2.28821799751,2.304581733269,0.2351725620026));
#13220=CARTESIAN_POINT('Ctrl Pts',(-2.013422824415,2.212859511047,-0.8092814225342));
#13221=CARTESIAN_POINT('Ctrl Pts',(-1.719918344731,2.166998399936,-1.222282346756));
#13222=CARTESIAN_POINT('Ctrl Pts',(1.950430605956,6.354663466539,-0.9261325432193));
#13223=CARTESIAN_POINT('Ctrl Pts',(2.172821161573,6.308802355428,-0.4577791208848));
#13224=CARTESIAN_POINT('Ctrl Pts',(2.264152887855,6.217080133205,0.6435937599656));
#13225=CARTESIAN_POINT('Ctrl Pts',(1.277006047232,6.079496799872,1.977757564583));
#13226=CARTESIAN_POINT('Ctrl Pts',(-0.3449220802747,5.941913466539,2.328671646129));
#13227=CARTESIAN_POINT('Ctrl Pts',(-1.795394938182,5.804330133205,1.522614969079));
#13228=CARTESIAN_POINT('Ctrl Pts',(-2.353760772811,5.666746799872,-0.04005948877329));
#13229=CARTESIAN_POINT('Ctrl Pts',(-1.742547832982,5.529163466539,-1.582818737658));
#13230=CARTESIAN_POINT('Ctrl Pts',(-0.2654712401003,5.391580133205,-2.339084449417));
#13231=CARTESIAN_POINT('Ctrl Pts',(1.343517262312,5.253996799872,-1.933067946727));
#13232=CARTESIAN_POINT('Ctrl Pts',(2.284917434461,5.116413466539,-0.5665180648611));
#13233=CARTESIAN_POINT('Ctrl Pts',(2.0909514892,4.978830133205,1.081532380318));
#13234=CARTESIAN_POINT('Ctrl Pts',(0.8580002821075,4.841246799872,2.192173789215));
#13235=CARTESIAN_POINT('Ctrl Pts',(-0.8012877593092,4.703663466539,2.213532998868));
#13236=CARTESIAN_POINT('Ctrl Pts',(-2.0624191861,4.566080133205,1.134996700628));
#13237=CARTESIAN_POINT('Ctrl Pts',(-2.298742942253,4.428496799872,-0.5075148224894));
#13238=CARTESIAN_POINT('Ctrl Pts',(-1.392830718655,4.290913466539,-1.897844303107));
#13239=CARTESIAN_POINT('Ctrl Pts',(0.2051734006369,4.153330133205,-2.345142700415));
#13240=CARTESIAN_POINT('Ctrl Pts',(1.701227695095,4.015746799872,-1.627149267617));
#13241=CARTESIAN_POINT('Ctrl Pts',(2.351948895778,3.878163466539,-0.1006320091092));
#13242=CARTESIAN_POINT('Ctrl Pts',(1.833996295711,3.740580133205,1.475888883674));
#13243=CARTESIAN_POINT('Ctrl Pts',(0.4047384263025,3.602996799872,2.319046618024));
#13244=CARTESIAN_POINT('Ctrl Pts',(-1.225632313532,3.465413466539,2.009879558143));
#13245=CARTESIAN_POINT('Ctrl Pts',(-2.246991364667,3.327830133205,0.7020115575811));
#13246=CARTESIAN_POINT('Ctrl Pts',(-2.151829574871,3.190246799872,-0.9546831311102));
#13247=CARTESIAN_POINT('Ctrl Pts',(-0.9874324899755,3.052663466539,-2.1369996253));
#13248=CARTESIAN_POINT('Ctrl Pts',(0.6676158875029,2.915080133205,-2.25744990367));
#13249=CARTESIAN_POINT('Ctrl Pts',(1.990928205287,2.777496799872,-1.256181908764));
#13250=CARTESIAN_POINT('Ctrl Pts',(2.324958115024,2.639913466539,0.3692753737369));
#13251=CARTESIAN_POINT('Ctrl Pts',(1.503719540172,2.502330133205,1.811250085609));
#13252=CARTESIAN_POINT('Ctrl Pts',(-0.06468764889537,2.364746799872,2.353188982004));
#13253=CARTESIAN_POINT('Ctrl Pts',(-1.601039452915,2.227163466539,1.725961210209));
#13254=CARTESIAN_POINT('Ctrl Pts',(-2.34151420154,2.089580133205,0.2406501016691));
#13255=CARTESIAN_POINT('Ctrl Pts',(-2.060318615711,1.997857910983,-0.8281308625178));
#13256=CARTESIAN_POINT('Ctrl Pts',(-1.759977954049,1.951996799872,-1.250751229269));
#13257=CARTESIAN_POINT('Ctrl Pts',(1.965062045595,6.316751913189,-0.9330800615582));
#13258=CARTESIAN_POINT('Ctrl Pts',(2.189120896398,6.270890802077,-0.461213217722));
#13259=CARTESIAN_POINT('Ctrl Pts',(2.281137760944,6.179168579855,0.6484217724168));
#13260=CARTESIAN_POINT('Ctrl Pts',(1.286585694332,6.041585246522,1.992594001388));
#13261=CARTESIAN_POINT('Ctrl Pts',(-0.3475095635628,5.904001913189,2.346140516093));
#13262=CARTESIAN_POINT('Ctrl Pts',(-1.808863355149,5.766418579855,1.534037087326));
#13263=CARTESIAN_POINT('Ctrl Pts',(-2.371417852518,5.628835246522,-0.04036000087055));
#13264=CARTESIAN_POINT('Ctrl Pts',(-1.755619809682,5.491251913189,-1.594692483255));
#13265=CARTESIAN_POINT('Ctrl Pts',(-0.2674627113239,5.353668579855,-2.356631432544));
#13266=CARTESIAN_POINT('Ctrl Pts',(1.353595852992,5.216085246522,-1.947569137845));
#13267=CARTESIAN_POINT('Ctrl Pts',(2.302058075825,5.078501913189,-0.570767882745));
#13268=CARTESIAN_POINT('Ctrl Pts',(2.106637066738,4.940918579855,1.089645653198));
#13269=CARTESIAN_POINT('Ctrl Pts',(0.8644366963533,4.803335246522,2.208618700598));
#13270=CARTESIAN_POINT('Ctrl Pts',(-0.8072987362944,4.665751913189,2.230138139478));
#13271=CARTESIAN_POINT('Ctrl Pts',(-2.077890724405,4.528168579855,1.143511043905));
#13272=CARTESIAN_POINT('Ctrl Pts',(-2.31598729768,4.390585246522,-0.5113220189456));
#13273=CARTESIAN_POINT('Ctrl Pts',(-1.403279241419,4.253001913189,-1.912081258926));
#13274=CARTESIAN_POINT('Ctrl Pts',(0.206712538824,4.115418579855,-2.362735130395));
#13275=CARTESIAN_POINT('Ctrl Pts',(1.713989702755,3.977835246522,-1.639355565149));
#13276=CARTESIAN_POINT('Ctrl Pts',(2.369592383424,3.840251913189,-0.1013869148015));
#13277=CARTESIAN_POINT('Ctrl Pts',(1.847754286391,3.702668579855,1.486960479376));
#13278=CARTESIAN_POINT('Ctrl Pts',(0.4077746306339,3.565085246522,2.336443284436));
#13279=CARTESIAN_POINT('Ctrl Pts',(-1.234826573077,3.427501913189,2.024956962767));
#13280=CARTESIAN_POINT('Ctrl Pts',(-2.263847498087,3.289918579855,0.7072777996607));
#13281=CARTESIAN_POINT('Ctrl Pts',(-2.167971838247,3.152335246522,-0.961844825848));
#13282=CARTESIAN_POINT('Ctrl Pts',(-0.9948398588049,3.014751913189,-2.153030639647));
#13283=CARTESIAN_POINT('Ctrl Pts',(0.6726241054473,2.877168579855,-2.274384493346));
#13284=CARTESIAN_POINT('Ctrl Pts',(2.005863443573,2.739585246522,-1.265605340552));
#13285=CARTESIAN_POINT('Ctrl Pts',(2.342399127393,2.602001913189,0.3720455468077));
#13286=CARTESIAN_POINT('Ctrl Pts',(1.514999911603,2.464418579855,1.824837442277));
#13287=CARTESIAN_POINT('Ctrl Pts',(-0.06517291272752,2.326835246522,2.370841772339));
#13288=CARTESIAN_POINT('Ctrl Pts',(-1.613049883864,2.189251913189,1.738908759939));
#13289=CARTESIAN_POINT('Ctrl Pts',(-2.359079411806,2.051668579855,0.2424553735028));
#13290=CARTESIAN_POINT('Ctrl Pts',(-2.075774396281,1.959946357633,-0.8343432069565));
#13291=CARTESIAN_POINT('Ctrl Pts',(-1.773180685345,1.914085246522,-1.260133922024));
#13292=CARTESIAN_POINT('Ctrl Pts',(-2.80488203134928,2.11666634473297,-0.494572811624998));
#13293=CARTESIAN_POINT('Ctrl Pts',(-2.80487937558295,2.14660584631654,-0.494558004365478));
#13294=CARTESIAN_POINT('Ctrl Pts',(-2.79983346453888,2.17665566318614,-0.493655688297967));
#13295=CARTESIAN_POINT('Ctrl Pts',(-2.7905135174355,2.2059245277796,-0.492002307694268));
#13296=CARTESIAN_POINT('Ctrl Pts',(-2.78143449325766,2.23443678502249,-0.490391667385945));
#13297=CARTESIAN_POINT('Ctrl Pts',(-2.76829948694453,2.26220798327608,-0.488068281113208));
#13298=CARTESIAN_POINT('Ctrl Pts',(-2.75185030367526,2.2883767040173,-0.485163523889622));
#13299=CARTESIAN_POINT('Ctrl Pts',(-2.73697041671003,2.31204885845072,-0.482535888313992));
#13300=CARTESIAN_POINT('Ctrl Pts',(-2.71937882394718,2.33440936083768,-0.479432564842254));
#13301=CARTESIAN_POINT('Ctrl Pts',(-2.69964797550406,2.35479239767097,-0.475954789776935));
#13302=CARTESIAN_POINT('Ctrl Pts',(-2.67769398815498,2.37747205759862,-0.472085162476968));
#13303=CARTESIAN_POINT('Ctrl Pts',(-2.65308669226524,2.39770433951941,-0.467748957240234));
#13304=CARTESIAN_POINT('Ctrl Pts',(-2.62668935647612,2.41451402502038,-0.463099122677085));
#13305=CARTESIAN_POINT('Ctrl Pts',(-2.59782850631059,2.43289246360406,-0.458015345295399));
#13306=CARTESIAN_POINT('Ctrl Pts',(-2.56682898609739,2.44717752991955,-0.452556858916761));
#13307=CARTESIAN_POINT('Ctrl Pts',(-2.53488055017212,2.45610210728703,-0.446934213906201));
#13308=CARTESIAN_POINT('Ctrl Pts',(-2.51095355439453,2.4627859501358,-0.442723272132987));
#13309=CARTESIAN_POINT('Ctrl Pts',(-2.4864958736503,2.46646307575719,-0.438420524025264));
#13310=CARTESIAN_POINT('Ctrl Pts',(-2.46201974870111,2.46661565567391,-0.434116553411453));
#13311=CARTESIAN_POINT('Ctrl Pts',(-2.4614874708036,2.46661897380198,-0.434022955734777));
#13312=CARTESIAN_POINT('Ctrl Pts',(-2.46095516857897,2.46662062601791,-0.433929353220448));
#13313=CARTESIAN_POINT('Ctrl Pts',(-2.46042284748648,2.46662060679558,-0.433835746825998));
#13314=CARTESIAN_POINT('Ctrl Pts',(-2.4341026224681,2.46661965636165,-0.429207447478404));
#13315=CARTESIAN_POINT('Ctrl Pts',(-2.4077358960525,2.46252740142272,-0.424569585932339));
#13316=CARTESIAN_POINT('Ctrl Pts',(-2.38198601504193,2.45495667506435,-0.420038577079773));
#13317=CARTESIAN_POINT('Ctrl Pts',(-2.35468695727497,2.44693047501666,-0.415234971488041));
#13318=CARTESIAN_POINT('Ctrl Pts',(-2.32808303963376,2.43499588080182,-0.410551788797338));
#13319=CARTESIAN_POINT('Ctrl Pts',(-2.30295408710686,2.41994167565776,-0.40612600330845));
#13320=CARTESIAN_POINT('Ctrl Pts',(-2.27843778078218,2.40525449343672,-0.401808118881841));
#13321=CARTESIAN_POINT('Ctrl Pts',(-2.2553269609863,2.38759986147607,-0.397735514989597));
#13322=CARTESIAN_POINT('Ctrl Pts',(-2.23431049879009,2.36773953428499,-0.39402922589206));
#13323=CARTESIAN_POINT('Ctrl Pts',(-2.23039092446436,2.3640355793647,-0.393338002247719));
#13324=CARTESIAN_POINT('Ctrl Pts',(-2.22654405866287,2.36025494368539,-0.392659495570005));
#13325=CARTESIAN_POINT('Ctrl Pts',(-2.22277416406729,2.35640260460539,-0.391994454672969));
#13326=CARTESIAN_POINT('Ctrl Pts',(-2.19954128922871,2.33266164596257,-0.387895981484488));
#13327=CARTESIAN_POINT('Ctrl Pts',(-2.17920592227961,2.306174071094,-0.384307040881674));
#13328=CARTESIAN_POINT('Ctrl Pts',(-2.16269258007162,2.27798421341354,-0.381390012556976));
#13329=CARTESIAN_POINT('Ctrl Pts',(-2.14410185480835,2.24624806377481,-0.378106021255483));
#13330=CARTESIAN_POINT('Ctrl Pts',(-2.13035431230019,2.21235423640297,-0.375673478333305));
#13331=CARTESIAN_POINT('Ctrl Pts',(-2.1227482802833,2.17772617536897,-0.374320245893729));
#13332=CARTESIAN_POINT('Ctrl Pts',(-2.11831275250703,2.15753250195116,-0.373531095905909));
#13333=CARTESIAN_POINT('Ctrl Pts',(-2.11596549328742,2.13708792799894,-0.373108934523806));
#13334=CARTESIAN_POINT('Ctrl Pts',(-2.11596363797559,2.11666691256093,-0.373098826465249));
#13335=CARTESIAN_POINT('Ctrl Pts',(-2.723241031212,2.083418579855,0.7501055518504));
#13336=CARTESIAN_POINT('Ctrl Pts',(-2.90336253938,2.037557468744,0.09617854059695));
#13337=CARTESIAN_POINT('Ctrl Pts',(-2.770829284715,1.945835246522,-1.343530217087));
#13338=CARTESIAN_POINT('Ctrl Pts',(-1.195947740385,1.808251913189,-2.838156522639));
#13339=CARTESIAN_POINT('Ctrl Pts',(0.9733915155363,1.670668579855,-2.921802275403));
#13340=CARTESIAN_POINT('Ctrl Pts',(2.659003940873,1.533085246522,-1.553807235173));
#13341=CARTESIAN_POINT('Ctrl Pts',(3.023382251462,1.395501913189,0.586319405716));
#13342=CARTESIAN_POINT('Ctrl Pts',(1.885450495222,1.257918579855,2.435092627868));
#13343=CARTESIAN_POINT('Ctrl Pts',(-0.1893529006074,1.120335246522,3.07388193938));
#13344=CARTESIAN_POINT('Ctrl Pts',(-2.1700678844,0.9827519131886,2.185270885497));
#13345=CARTESIAN_POINT('Ctrl Pts',(-3.072484926538,0.8451685798553,0.2108079169741));
#13346=CARTESIAN_POINT('Ctrl Pts',(-2.448196776368,0.7075852465219,-1.868404715163));
#13347=CARTESIAN_POINT('Ctrl Pts',(-0.6074096414087,0.5700019131886,-3.019214656103));
#13348=CARTESIAN_POINT('Ctrl Pts',(1.535196862268,0.4324185798553,-2.669789170172));
#13349=CARTESIAN_POINT('Ctrl Pts',(2.914970315305,0.2948352465219,-0.9937563478226));
#13350=CARTESIAN_POINT('Ctrl Pts',(2.846306923502,0.1572519131886,1.176069944827));
#13351=CARTESIAN_POINT('Ctrl Pts',(1.363325245947,0.01966857985526,2.761511885139));
#13352=CARTESIAN_POINT('Ctrl Pts',(-0.7970871784129,-0.1179147534781,2.974769847899));
#13353=CARTESIAN_POINT('Ctrl Pts',(-2.561430239181,-0.2554980868114,1.70987682241));
#13354=CARTESIAN_POINT('Ctrl Pts',(-3.053009075134,-0.3930814201447,-0.4046470129032));
#13355=CARTESIAN_POINT('Ctrl Pts',(-2.02756017042,-0.5306647534781,-2.318103400039));
#13356=CARTESIAN_POINT('Ctrl Pts',(0.005375102551742,-0.6682480868114,-3.079703675251));
#13357=CARTESIAN_POINT('Ctrl Pts',(2.035639508015,-0.8058314201447,-2.311011770959));
#13358=CARTESIAN_POINT('Ctrl Pts',(3.054402959379,-0.9434147534781,-0.3939875596977));
#13359=CARTESIAN_POINT('Ctrl Pts',(2.55544604064,-1.080998086811,1.718807474687));
#13360=CARTESIAN_POINT('Ctrl Pts',(0.7866984730786,-1.218581420145,2.977534043191));
#13361=CARTESIAN_POINT('Ctrl Pts',(-1.372956547484,-1.356164753478,2.756736298041));
#13362=CARTESIAN_POINT('Ctrl Pts',(-2.850394340374,-1.493748086811,1.166126828691));
#13363=CARTESIAN_POINT('Ctrl Pts',(-2.911485537975,-1.631331420145,-1.003923625649));
#13364=CARTESIAN_POINT('Ctrl Pts',(-1.525861343972,-1.768914753478,-2.67513850868));
#13365=CARTESIAN_POINT('Ctrl Pts',(0.6179193574188,-1.906498086811,-3.017050753102));
#13366=CARTESIAN_POINT('Ctrl Pts',(2.454799386092,-2.044081420145,-1.859941778329));
#13367=CARTESIAN_POINT('Ctrl Pts',(3.071373658657,-2.181664753478,0.2218833436086));
#13368=CARTESIAN_POINT('Ctrl Pts',(2.466296445201,-2.2733869757,1.534974329146));
#13369=CARTESIAN_POINT('Ctrl Pts',(1.983343137733,-2.319248086811,2.011230979028));
#13370=CARTESIAN_POINT('Ctrl Pts',(-2.738856610305,2.121330133205,0.7544067989448));
#13371=CARTESIAN_POINT('Ctrl Pts',(-2.920010969265,2.075469022094,0.09673004653804));
#13372=CARTESIAN_POINT('Ctrl Pts',(-2.786717743854,1.983746799872,-1.35123427344));
#13373=CARTESIAN_POINT('Ctrl Pts',(-1.202805530906,1.846163466539,-2.854431048893));
#13374=CARTESIAN_POINT('Ctrl Pts',(0.9789731265745,1.708580133205,-2.938556442222));
#13375=CARTESIAN_POINT('Ctrl Pts',(2.674251172341,1.570996799872,-1.562717059716));
#13376=CARTESIAN_POINT('Ctrl Pts',(3.040718897075,1.433413466539,0.5896814720732));
#13377=CARTESIAN_POINT('Ctrl Pts',(1.896262024938,1.295830133205,2.449055909521));
#13378=CARTESIAN_POINT('Ctrl Pts',(-0.19043868595,1.158246799872,3.091508159754));
#13379=CARTESIAN_POINT('Ctrl Pts',(-2.182511464053,1.020663466539,2.197801642033));
#13380=CARTESIAN_POINT('Ctrl Pts',(-3.090103136176,0.8830801332053,0.2120167294381));
#13381=CARTESIAN_POINT('Ctrl Pts',(-2.462235199687,0.745496799872,-1.879118501153));
#13382=CARTESIAN_POINT('Ctrl Pts',(-0.610892643166,0.6079134665387,-3.036527403935));
#13383=CARTESIAN_POINT('Ctrl Pts',(1.543999971413,0.4703301332053,-2.685098246184));
#13384=CARTESIAN_POINT('Ctrl Pts',(2.931685306373,0.332746799872,-0.9994547346604));
#13385=CARTESIAN_POINT('Ctrl Pts',(2.862628185696,0.1951634665387,1.18281375231));
#13386=CARTESIAN_POINT('Ctrl Pts',(1.37114281074,0.05758013320533,2.777346916547));
#13387=CARTESIAN_POINT('Ctrl Pts',(-0.8016578270393,-0.08000320012801,2.991827740796));
#13388=CARTESIAN_POINT('Ctrl Pts',(-2.57611796459,-0.2175865334613,1.719681579482));
#13389=CARTESIAN_POINT('Ctrl Pts',(-3.070515606557,-0.3551698667947,-0.4069673354021));
#13390=CARTESIAN_POINT('Ctrl Pts',(-2.03918658389,-0.492753200128,-2.331395843335));
#13391=CARTESIAN_POINT('Ctrl Pts',(0.005405924406315,-0.6303365334613,-3.097363278559));
#13392=CARTESIAN_POINT('Ctrl Pts',(2.047312249934,-0.7679198667947,-2.324263549512));
#13393=CARTESIAN_POINT('Ctrl Pts',(3.071917483598,-0.905503200128,-0.396246758876));
#13394=CARTESIAN_POINT('Ctrl Pts',(2.570099451523,-1.043086533461,1.728663441808));
#13395=CARTESIAN_POINT('Ctrl Pts',(0.7912095509038,-1.180669866795,2.994607786506));
#13396=CARTESIAN_POINT('Ctrl Pts',(-1.380829339981,-1.318253200128,2.772543945329));
#13397=CARTESIAN_POINT('Ctrl Pts',(-2.866739040589,-1.455836533461,1.172813620464));
#13398=CARTESIAN_POINT('Ctrl Pts',(-2.928180546671,-1.593419866795,-1.009680313581));
#13399=CARTESIAN_POINT('Ctrl Pts',(-1.53461092149,-1.731003200128,-2.690478258812));
#13400=CARTESIAN_POINT('Ctrl Pts',(0.6214626238752,-1.868586533461,-3.034351092706));
#13401=CARTESIAN_POINT('Ctrl Pts',(2.468875670024,-2.006169866795,-1.870607036239));
#13402=CARTESIAN_POINT('Ctrl Pts',(3.088985496074,-2.143753200128,0.2231556646635));
#13403=CARTESIAN_POINT('Ctrl Pts',(2.480438655444,-2.23547542235,1.543776162244));
#13404=CARTESIAN_POINT('Ctrl Pts',(1.994716002375,-2.281336533461,2.022763757826));
#13405=CARTESIAN_POINT('Ctrl Pts',(-2.786237260851,2.336331733269,0.7674576044437));
#13406=CARTESIAN_POINT('Ctrl Pts',(-2.970525486456,2.290470622158,0.09840342093635));
#13407=CARTESIAN_POINT('Ctrl Pts',(-2.834926364595,2.198748399936,-1.374609852386));
#13408=CARTESIAN_POINT('Ctrl Pts',(-1.223613377626,2.061165066603,-2.903811071025));
#13409=CARTESIAN_POINT('Ctrl Pts',(0.9959088009101,1.923581733269,-2.989391785472));
#13410=CARTESIAN_POINT('Ctrl Pts',(2.720514185816,1.785998399936,-1.589751169728));
#13411=CARTESIAN_POINT('Ctrl Pts',(3.093321592276,1.648415066603,0.5998826237716));
#13412=CARTESIAN_POINT('Ctrl Pts',(1.929066271794,1.510831733269,2.491423173941));
#13413=CARTESIAN_POINT('Ctrl Pts',(-0.193733166134,1.373248399936,3.144989480107));
#13414=CARTESIAN_POINT('Ctrl Pts',(-2.220267662242,1.235665066603,2.235822351543));
#13415=CARTESIAN_POINT('Ctrl Pts',(-3.143560150426,1.098081733269,0.2156844974145));
#13416=CARTESIAN_POINT('Ctrl Pts',(-2.504830458278,0.960498399936,-1.911626174867));
#13417=CARTESIAN_POINT('Ctrl Pts',(-0.6214607359745,0.8229150666027,-3.089057588706));
#13418=CARTESIAN_POINT('Ctrl Pts',(1.570710286518,0.6853317332693,-2.731548907824));
#13419=CARTESIAN_POINT('Ctrl Pts',(2.982401782909,0.547748399936,-1.016744729084));
#13420=CARTESIAN_POINT('Ctrl Pts',(2.9121500136,0.4101650666027,1.203275752711));
#13421=CARTESIAN_POINT('Ctrl Pts',(1.394862795977,0.2725817332693,2.825393427343));
#13422=CARTESIAN_POINT('Ctrl Pts',(-0.8155260482588,0.134998399936,3.043584646998));
#13423=CARTESIAN_POINT('Ctrl Pts',(-2.620683329782,-0.002584933397334,1.749431085776));
#13424=CARTESIAN_POINT('Ctrl Pts',(-3.123633767764,-0.1401682667307,-0.4140076371944));
#13425=CARTESIAN_POINT('Ctrl Pts',(-2.074463343749,-0.277751600064,-2.371727656005));
#13426=CARTESIAN_POINT('Ctrl Pts',(0.005499443802035,-0.4153349333973,-3.150945889114));
#13427=CARTESIAN_POINT('Ctrl Pts',(2.082729579161,-0.5529182667307,-2.364471977585));
#13428=CARTESIAN_POINT('Ctrl Pts',(3.125059896475,-0.690501600064,-0.4031016008351));
#13429=CARTESIAN_POINT('Ctrl Pts',(2.614560699886,-0.8280849333973,1.758568329176));
#13430=CARTESIAN_POINT('Ctrl Pts',(0.804897022931,-0.9656682667307,3.046412785907));
#13431=CARTESIAN_POINT('Ctrl Pts',(-1.404716896626,-1.103251600064,2.820507367475));
#13432=CARTESIAN_POINT('Ctrl Pts',(-2.916331983928,-1.240834933397,1.193102624313));
#13433=CARTESIAN_POINT('Ctrl Pts',(-2.978836392872,-1.378418266731,-1.027147204663));
#13434=CARTESIAN_POINT('Ctrl Pts',(-1.561158811409,-1.516001600064,-2.737021991588));
#13435=CARTESIAN_POINT('Ctrl Pts',(0.6322135712956,-1.653584933397,-3.086843628539));
#13436=CARTESIAN_POINT('Ctrl Pts',(2.511585804947,-1.791168266731,-1.902967466485));
#13437=CARTESIAN_POINT('Ctrl Pts',(3.142423175791,-1.928751600064,0.227016129839));
#13438=CARTESIAN_POINT('Ctrl Pts',(2.523348823392,-2.020473822286,1.570482605578));
#13439=CARTESIAN_POINT('Ctrl Pts',(2.029223446646,-2.066334933397,2.057756412201));
#13440=CARTESIAN_POINT('Ctrl Pts',(-2.410238510585,2.726333333333,0.663890293717));
#13441=CARTESIAN_POINT('Ctrl Pts',(-2.569657302604,2.680472222222,0.08512401942456));
#13442=CARTESIAN_POINT('Ctrl Pts',(-2.452357089121,2.58875,-1.18910821049));
#13443=CARTESIAN_POINT('Ctrl Pts',(-1.058488494954,2.451166666667,-2.511945902522));
#13444=CARTESIAN_POINT('Ctrl Pts',(0.8615123265745,2.313583333333,-2.585977621436));
#13445=CARTESIAN_POINT('Ctrl Pts',(2.353384670925,2.176,-1.375216513455));
#13446=CARTESIAN_POINT('Ctrl Pts',(2.675882248826,2.038416666667,0.5189293180307));
#13447=CARTESIAN_POINT('Ctrl Pts',(1.668741525741,1.900833333333,2.155209164837));
#13448=CARTESIAN_POINT('Ctrl Pts',(-0.1675891512739,1.76325,2.720577628778));
#13449=CARTESIAN_POINT('Ctrl Pts',(-1.92064570327,1.625666666667,1.934101309402));
#13450=CARTESIAN_POINT('Ctrl Pts',(-2.719341185102,1.488083333333,0.1865781816606));
#13451=CARTESIAN_POINT('Ctrl Pts',(-2.166807155247,1.3505,-1.653654945056));
#13452=CARTESIAN_POINT('Ctrl Pts',(-0.5375954947229,1.212916666667,-2.672193666465));
#13453=CARTESIAN_POINT('Ctrl Pts',(1.358745170317,1.075333333333,-2.362930272913));
#13454=CARTESIAN_POINT('Ctrl Pts',(2.579930909764,0.93775,-0.8795364759154));
#13455=CARTESIAN_POINT('Ctrl Pts',(2.519159516672,0.8001666666667,1.040895403556));
#13456=CARTESIAN_POINT('Ctrl Pts',(1.206628048187,0.6625833333333,2.444110608175));
#13457=CARTESIAN_POINT('Ctrl Pts',(-0.7054719694972,0.525,2.632857233479));
#13458=CARTESIAN_POINT('Ctrl Pts',(-2.267025846736,0.3874166666667,1.513347852245));
#13459=CARTESIAN_POINT('Ctrl Pts',(-2.702103839402,0.2498333333333,-0.3581378961739));
#13460=CARTESIAN_POINT('Ctrl Pts',(-1.794517469906,0.11225,-2.05166638658));
#13461=CARTESIAN_POINT('Ctrl Pts',(0.004757301693121,-0.02533333333332,
-2.725730228873));
#13462=CARTESIAN_POINT('Ctrl Pts',(1.801668188622,-0.1629166666667,-2.045389851629));
#13463=CARTESIAN_POINT('Ctrl Pts',(2.703337514074,-0.3005,-0.3487036138892));
#13464=CARTESIAN_POINT('Ctrl Pts',(2.261729457025,-0.4380833333333,1.521252037661));
#13465=CARTESIAN_POINT('Ctrl Pts',(0.6962773159997,-0.5756666666667,2.63530371907));
#13466=CARTESIAN_POINT('Ctrl Pts',(-1.215152351987,-0.71325,2.439883915127));
#13467=CARTESIAN_POINT('Ctrl Pts',(-2.52277713606,-0.8508333333333,1.032095124347));
#13468=CARTESIAN_POINT('Ctrl Pts',(-2.576846664034,-0.9884166666667,-0.8885351522298));
#13469=CARTESIAN_POINT('Ctrl Pts',(-1.350482653171,-1.126,-2.367664771818));
#13470=CARTESIAN_POINT('Ctrl Pts',(0.5468972502313,-1.263583333333,-2.670278477069));
#13471=CARTESIAN_POINT('Ctrl Pts',(2.172650877504,-1.401166666667,-1.64616471704));
#13472=CARTESIAN_POINT('Ctrl Pts',(2.718357643575,-1.53875,0.1963806264277));
#13473=CARTESIAN_POINT('Ctrl Pts',(2.182826493363,-1.630472222222,1.358548214596));
#13474=CARTESIAN_POINT('Ctrl Pts',(1.755382632488,-1.676333333333,1.780065114977));
#13475=CARTESIAN_POINT('Ctrl Pts',(-2.03423976032,2.336331733269,0.5603229829904));
#13476=CARTESIAN_POINT('Ctrl Pts',(-2.168789118751,2.290470622158,0.07184461791278));
#13477=CARTESIAN_POINT('Ctrl Pts',(-2.069787813647,2.198748399936,-1.003606568594));
#13478=CARTESIAN_POINT('Ctrl Pts',(-0.8933636122811,2.061165066603,-2.120080734019));
#13479=CARTESIAN_POINT('Ctrl Pts',(0.7271158522389,1.923581733269,-2.1825634574));
#13480=CARTESIAN_POINT('Ctrl Pts',(1.986255156035,1.785998399936,-1.160681857182));
#13481=CARTESIAN_POINT('Ctrl Pts',(2.258442905376,1.648415066603,0.4379760122899));
#13482=CARTESIAN_POINT('Ctrl Pts',(1.408416779688,1.510831733269,1.818995155733));
#13483=CARTESIAN_POINT('Ctrl Pts',(-0.1414451364138,1.373248399936,2.29616577745));
#13484=CARTESIAN_POINT('Ctrl Pts',(-1.621023744297,1.235665066603,1.632380267261));
#13485=CARTESIAN_POINT('Ctrl Pts',(-2.295122219778,1.098081733269,0.1574718659068));
#13486=CARTESIAN_POINT('Ctrl Pts',(-1.828783852216,0.960498399936,-1.395683715246));
#13487=CARTESIAN_POINT('Ctrl Pts',(-0.4537302534712,0.8229150666027,-2.255329744224));
#13488=CARTESIAN_POINT('Ctrl Pts',(1.146780054116,0.6853317332693,-1.994311638003));
#13489=CARTESIAN_POINT('Ctrl Pts',(2.177460036619,0.547748399936,-0.7423282227468));
#13490=CARTESIAN_POINT('Ctrl Pts',(2.126169019745,0.4101650666027,0.8785150544019));
#13491=CARTESIAN_POINT('Ctrl Pts',(1.018393300397,0.2725817332693,2.062827789006));
#13492=CARTESIAN_POINT('Ctrl Pts',(-0.5954178907355,0.134998399936,2.22212981996));
#13493=CARTESIAN_POINT('Ctrl Pts',(-1.913368363691,-0.002584933397335,1.277264618713));
#13494=CARTESIAN_POINT('Ctrl Pts',(-2.28057391104,-0.1401682667307,-0.3022681551533));
#13495=CARTESIAN_POINT('Ctrl Pts',(-1.514571596064,-0.277751600064,-1.731605117154));
#13496=CARTESIAN_POINT('Ctrl Pts',(0.004015159584192,-0.4153349333973,-2.300514568631));
#13497=CARTESIAN_POINT('Ctrl Pts',(1.520606798084,-0.5529182667307,-1.726307725673));
#13498=CARTESIAN_POINT('Ctrl Pts',(2.281615131673,-0.690501600064,-0.2943056269432));
#13499=CARTESIAN_POINT('Ctrl Pts',(1.908898214165,-0.8280849333973,1.283935746146));
#13500=CARTESIAN_POINT('Ctrl Pts',(0.5876576090685,-0.9656682667307,2.224194652233));
#13501=CARTESIAN_POINT('Ctrl Pts',(-1.025587807349,-1.103251600064,2.059260462779));
#13502=CARTESIAN_POINT('Ctrl Pts',(-2.129222288193,-1.240834933397,0.8710876243819));
#13503=CARTESIAN_POINT('Ctrl Pts',(-2.174856935197,-1.378418266731,-0.7499230997967));
#13504=CARTESIAN_POINT('Ctrl Pts',(-1.139806494933,-1.516001600064,-1.998307552049));
#13505=CARTESIAN_POINT('Ctrl Pts',(0.4615809291669,-1.653584933397,-2.2537133256));
#13506=CARTESIAN_POINT('Ctrl Pts',(1.833715950062,-1.791168266731,-1.389361967594));
#13507=CARTESIAN_POINT('Ctrl Pts',(2.294292111359,-1.928751600064,0.1657451230163));
#13508=CARTESIAN_POINT('Ctrl Pts',(1.842304163333,-2.020473822286,1.146613823613));
#13509=CARTESIAN_POINT('Ctrl Pts',(1.48154181833,-2.066334933397,1.502373817754));
#13510=CARTESIAN_POINT('Ctrl Pts',(-2.081620410866,2.121330133205,0.5733737884892));
#13511=CARTESIAN_POINT('Ctrl Pts',(-2.219303635942,2.075469022094,0.07351799231108));
#13512=CARTESIAN_POINT('Ctrl Pts',(-2.117996434389,1.983746799872,-1.02698214754));
#13513=CARTESIAN_POINT('Ctrl Pts',(-0.9141714590009,1.846163466539,-2.169460756152));
#13514=CARTESIAN_POINT('Ctrl Pts',(0.7440515265746,1.708580133205,-2.233398800651));
#13515=CARTESIAN_POINT('Ctrl Pts',(2.03251816951,1.570996799872,-1.187715967194));
#13516=CARTESIAN_POINT('Ctrl Pts',(2.311045600577,1.433413466539,0.4481771639882));
#13517=CARTESIAN_POINT('Ctrl Pts',(1.441221026544,1.295830133205,1.861362420153));
#13518=CARTESIAN_POINT('Ctrl Pts',(-0.1447396165978,1.158246799872,2.349647097803));
#13519=CARTESIAN_POINT('Ctrl Pts',(-1.658779942486,1.020663466539,1.670400976771));
#13520=CARTESIAN_POINT('Ctrl Pts',(-2.348579234028,0.8830801332053,0.1611396338832));
#13521=CARTESIAN_POINT('Ctrl Pts',(-1.871379110807,0.745496799872,-1.42819138896));
#13522=CARTESIAN_POINT('Ctrl Pts',(-0.4642983462798,0.6079134665387,-2.307859928994));
#13523=CARTESIAN_POINT('Ctrl Pts',(1.17349036922,0.4703301332053,-2.040762299642));
#13524=CARTESIAN_POINT('Ctrl Pts',(2.228176513155,0.332746799872,-0.7596182171705));
#13525=CARTESIAN_POINT('Ctrl Pts',(2.175690847649,0.1951634665387,0.8989770548032));
#13526=CARTESIAN_POINT('Ctrl Pts',(1.042113285635,0.05758013320533,2.110874299803));
#13527=CARTESIAN_POINT('Ctrl Pts',(-0.6092861119551,-0.08000320012801,2.273886726162));
#13528=CARTESIAN_POINT('Ctrl Pts',(-1.957933728882,-0.2175865334613,1.307014125008));
#13529=CARTESIAN_POINT('Ctrl Pts',(-2.333692072247,-0.3551698667947,-0.3093084569456));
#13530=CARTESIAN_POINT('Ctrl Pts',(-1.549848355923,-0.492753200128,-1.771936929824));
#13531=CARTESIAN_POINT('Ctrl Pts',(0.004108678979917,-0.6303365334613,-2.354097179186));
#13532=CARTESIAN_POINT('Ctrl Pts',(1.556024127311,-0.7679198667947,-1.766516153745));
#13533=CARTESIAN_POINT('Ctrl Pts',(2.33475754455,-0.905503200128,-0.3011604689023));
#13534=CARTESIAN_POINT('Ctrl Pts',(1.953359462527,-1.043086533461,1.313840633513));
#13535=CARTESIAN_POINT('Ctrl Pts',(0.6013450810956,-1.180669866795,2.275999651633));
#13536=CARTESIAN_POINT('Ctrl Pts',(-1.049475363994,-1.318253200128,2.107223884925));
#13537=CARTESIAN_POINT('Ctrl Pts',(-2.178815231532,-1.455836533461,0.8913766282303));
#13538=CARTESIAN_POINT('Ctrl Pts',(-2.225512781398,-1.593419866795,-0.7673899908785));
#13539=CARTESIAN_POINT('Ctrl Pts',(-1.166354384852,-1.731003200128,-2.044851284825));
#13540=CARTESIAN_POINT('Ctrl Pts',(0.4723318765873,-1.868586533461,-2.306205861433));
#13541=CARTESIAN_POINT('Ctrl Pts',(1.876426084985,-2.006169866795,-1.42172239784));
#13542=CARTESIAN_POINT('Ctrl Pts',(2.347729791075,-2.143753200128,0.1696055881918));
#13543=CARTESIAN_POINT('Ctrl Pts',(1.885214331281,-2.23547542235,1.173320266948));
#13544=CARTESIAN_POINT('Ctrl Pts',(1.516049262601,-2.281336533461,1.537366472129));
#13545=CARTESIAN_POINT('Ctrl Pts',(-2.097235989958,2.083418579855,0.5776750355837));
#13546=CARTESIAN_POINT('Ctrl Pts',(-2.235952065827,2.037557468744,0.07406949825217));
#13547=CARTESIAN_POINT('Ctrl Pts',(-2.133884893527,1.945835246522,-1.034686203893));
#13548=CARTESIAN_POINT('Ctrl Pts',(-0.9210292495221,1.808251913189,-2.185735282405));
#13549=CARTESIAN_POINT('Ctrl Pts',(0.7496331376127,1.670668579855,-2.25015296747));
#13550=CARTESIAN_POINT('Ctrl Pts',(2.047765400978,1.533085246522,-1.196625791736));
#13551=CARTESIAN_POINT('Ctrl Pts',(2.328382246189,1.395501913189,0.4515392303455));
#13552=CARTESIAN_POINT('Ctrl Pts',(1.452032556261,1.257918579855,1.875325701807));
#13553=CARTESIAN_POINT('Ctrl Pts',(-0.1458254019403,1.120335246522,2.367273318177));
#13554=CARTESIAN_POINT('Ctrl Pts',(-1.671223522139,0.9827519131886,1.682931733308));
#13555=CARTESIAN_POINT('Ctrl Pts',(-2.366197443666,0.8451685798553,0.1623484463472));
#13556=CARTESIAN_POINT('Ctrl Pts',(-1.885417534126,0.7075852465219,-1.43890517495));
#13557=CARTESIAN_POINT('Ctrl Pts',(-0.4677813480371,0.5700019131886,-2.325172676827));
#13558=CARTESIAN_POINT('Ctrl Pts',(1.182293478365,0.4324185798553,-2.056071375655));
#13559=CARTESIAN_POINT('Ctrl Pts',(2.244891504223,0.2948352465219,-0.7653166040083));
#13560=CARTESIAN_POINT('Ctrl Pts',(2.192012109843,0.1572519131886,0.9057208622855));
#13561=CARTESIAN_POINT('Ctrl Pts',(1.049930850427,0.01966857985526,2.12670933121));
#13562=CARTESIAN_POINT('Ctrl Pts',(-0.6138567605814,-0.1179147534781,2.290944619059));
#13563=CARTESIAN_POINT('Ctrl Pts',(-1.972621454292,-0.2554980868114,1.31681888208));
#13564=CARTESIAN_POINT('Ctrl Pts',(-2.35119860367,-0.3930814201447,-0.3116287794445));
#13565=CARTESIAN_POINT('Ctrl Pts',(-1.561474769393,-0.5306647534781,-1.785229373121));
#13566=CARTESIAN_POINT('Ctrl Pts',(0.004139500834489,-0.6682480868114,-2.371756782494));
#13567=CARTESIAN_POINT('Ctrl Pts',(1.56769686923,-0.8058314201447,-1.779767932299));
#13568=CARTESIAN_POINT('Ctrl Pts',(2.352272068769,-0.9434147534781,-0.3034196680806));
#13569=CARTESIAN_POINT('Ctrl Pts',(1.968012873411,-1.080998086811,1.323696600635));
#13570=CARTESIAN_POINT('Ctrl Pts',(0.6058561589209,-1.218581420145,2.293073394949));
#13571=CARTESIAN_POINT('Ctrl Pts',(-1.057348156491,-1.356164753478,2.123031532212));
#13572=CARTESIAN_POINT('Ctrl Pts',(-2.195159931747,-1.493748086811,0.8980634200042));
#13573=CARTESIAN_POINT('Ctrl Pts',(-2.242207790093,-1.631331420145,-0.7731466788102));
#13574=CARTESIAN_POINT('Ctrl Pts',(-1.175103962369,-1.768914753478,-2.060191034956));
#13575=CARTESIAN_POINT('Ctrl Pts',(0.4758751430437,-1.906498086811,-2.323506201036));
#13576=CARTESIAN_POINT('Ctrl Pts',(1.890502368917,-2.044081420145,-1.43238765575));
#13577=CARTESIAN_POINT('Ctrl Pts',(2.365341628493,-2.181664753478,0.1708779092467));
#13578=CARTESIAN_POINT('Ctrl Pts',(1.899356541525,-2.2733869757,1.182122100046));
#13579=CARTESIAN_POINT('Ctrl Pts',(1.527422127243,-2.319248086811,1.548899250927));
#13580=CARTESIAN_POINT('',(2.01902946446485,-2.11666642077307,0.73486384668651));
#13581=CARTESIAN_POINT('Ctrl Pts',(-2.1159627305594,2.11666642077307,-0.373103972679151));
#13582=CARTESIAN_POINT('Ctrl Pts',(-2.09791744924042,2.10732932202772,-0.476586603307615));
#13583=CARTESIAN_POINT('Ctrl Pts',(-2.07240856203006,2.09799224087489,-0.578864236800211));
#13584=CARTESIAN_POINT('Ctrl Pts',(-2.03952544136795,2.0886551715116,-0.678701259971635));
#13585=CARTESIAN_POINT('Ctrl Pts',(-2.01029652232723,2.08035570239182,-0.767443697087925));
#13586=CARTESIAN_POINT('Ctrl Pts',(-1.97524204365226,2.07205624258692,-0.854257078451053));
#13587=CARTESIAN_POINT('Ctrl Pts',(-1.93445881079141,2.06375678802135,-0.93827986748618));
#13588=CARTESIAN_POINT('Ctrl Pts',(-1.89504922115652,2.05573687209811,-1.01947263724898));
#13589=CARTESIAN_POINT('Ctrl Pts',(-1.8502908018872,2.04771696106718,-1.09805921260102));
#13590=CARTESIAN_POINT('Ctrl Pts',(-1.80075999246287,2.0396970512512,-1.17349099183197));
#13591=CARTESIAN_POINT('Ctrl Pts',(-1.74049142569068,2.02993850953002,-1.26527558562648));
#13592=CARTESIAN_POINT('Ctrl Pts',(-1.67317186324321,2.02017988192998,-1.35238096779209));
#13593=CARTESIAN_POINT('Ctrl Pts',(-1.59973693945821,2.01042122840127,-1.43398501440707));
#13594=CARTESIAN_POINT('Ctrl Pts',(-1.52530346600026,2.00052987914978,-1.51669869237808));
#13595=CARTESIAN_POINT('Ctrl Pts',(-1.44458628575752,1.99063850325969,-1.59376141933641));
#13596=CARTESIAN_POINT('Ctrl Pts',(-1.3585161844784,1.9807471631603,-1.66428745788304));
#13597=CARTESIAN_POINT('Ctrl Pts',(-1.3062486076442,1.97474047360196,-1.70711563031186));
#13598=CARTESIAN_POINT('Ctrl Pts',(-1.25200622931957,1.96873379724231,-1.74753260324364));
#13599=CARTESIAN_POINT('Ctrl Pts',(-1.19599201792712,1.96272714806199,-1.78533235701608));
#13600=CARTESIAN_POINT('Ctrl Pts',(-1.11297034403313,1.95382437040884,-1.84135740410602));
#13601=CARTESIAN_POINT('Ctrl Pts',(-1.02600255192884,1.94492160418517,-1.89166253407849));
#13602=CARTESIAN_POINT('Ctrl Pts',(-0.935879106074206,1.93601884024483,
-1.93547516733291));
#13603=CARTESIAN_POINT('Ctrl Pts',(-0.902630932934798,1.9327344492176,-1.95163844207593));
#13604=CARTESIAN_POINT('Ctrl Pts',(-0.868953602670152,1.92945005850113,
-1.96691847080026));
#13605=CARTESIAN_POINT('Ctrl Pts',(-0.834887819739237,1.92616566763619,
-1.98127795335741));
#13606=CARTESIAN_POINT('Ctrl Pts',(-0.742544771603072,1.91726257962103,
-2.02020259488623));
#13607=CARTESIAN_POINT('Ctrl Pts',(-0.647346424999575,1.90835949051486,
-2.05235929784953));
#13608=CARTESIAN_POINT('Ctrl Pts',(-0.550392479691278,1.89945639117047,
-2.07769736257899));
#13609=CARTESIAN_POINT('Ctrl Pts',(-0.500666710376223,1.89489016683808,
-2.09069275701725));
#13610=CARTESIAN_POINT('Ctrl Pts',(-0.450479375516837,1.89032393981257,
-2.1018953643128));
#13611=CARTESIAN_POINT('Ctrl Pts',(-0.399979430919417,1.88575770885988,
-2.11130361223012));
#13612=CARTESIAN_POINT('Ctrl Pts',(-0.28761302935216,1.87559748106223,-2.13223771368211));
#13613=CARTESIAN_POINT('Ctrl Pts',(-0.173596384538557,1.86543719671815,
-2.14431302429515));
#13614=CARTESIAN_POINT('Ctrl Pts',(-0.059331666635636,1.85527690565331,
-2.14749845845954));
#13615=CARTESIAN_POINT('Ctrl Pts',(0.0534748849115257,1.84524627311182,
-2.15064324234261));
#13616=CARTESIAN_POINT('Ctrl Pts',(0.166524593003937,1.83521563402004,-2.14512354089506));
#13617=CARTESIAN_POINT('Ctrl Pts',(0.278468664955484,1.82518503632032,-2.13085995349825));
#13618=CARTESIAN_POINT('Ctrl Pts',(0.339467829366259,1.81971928840212,-2.12308761774579));
#13619=CARTESIAN_POINT('Ctrl Pts',(0.400138589926789,1.81425355277422,-2.11271815102493));
#13620=CARTESIAN_POINT('Ctrl Pts',(0.460260570476484,1.80878783719352,-2.09973246983707));
#13621=CARTESIAN_POINT('Ctrl Pts',(0.534366335791568,1.80205084961594,-2.08372644618706));
#13622=CARTESIAN_POINT('Ctrl Pts',(0.607612372580839,1.79531386845014,-2.06374965831702));
#13623=CARTESIAN_POINT('Ctrl Pts',(0.679535519150437,1.78857688481004,-2.03978711598877));
#13624=CARTESIAN_POINT('Ctrl Pts',(0.784586812609899,1.77873681413512,-2.00478731152772));
#13625=CARTESIAN_POINT('Ctrl Pts',(0.886814383123217,1.7688967381816,-1.96128244214364));
#13626=CARTESIAN_POINT('Ctrl Pts',(0.985092375620573,1.75905662926039,-1.9101743840555));
#13627=CARTESIAN_POINT('Ctrl Pts',(1.07577295070114,1.74997721368467,-1.86301725374671));
#13628=CARTESIAN_POINT('Ctrl Pts',(1.16309051312948,1.74089777004143,-1.80938813864657));
#13629=CARTESIAN_POINT('Ctrl Pts',(1.24618512059533,1.73181827657948,-1.75002634145707));
#13630=CARTESIAN_POINT('Ctrl Pts',(1.36358913358838,1.71898989937323,-1.66615431388427));
#13631=CARTESIAN_POINT('Ctrl Pts',(1.47281388914806,1.70616159057245,-1.57067191622397));
#13632=CARTESIAN_POINT('Ctrl Pts',(1.57156518045832,1.69333330644984,-1.46538680864991));
#13633=CARTESIAN_POINT('Ctrl Pts',(1.66312630474595,1.68143906080139,-1.36776760091787));
#13634=CARTESIAN_POINT('Ctrl Pts',(1.7456841370641,1.66954483636822,-1.26172009680776));
#13635=CARTESIAN_POINT('Ctrl Pts',(1.81736534288417,1.65765059829595,-1.14866906455378));
#13636=CARTESIAN_POINT('Ctrl Pts',(1.82299436771583,1.65671656041675,-1.13979132511674));
#13637=CARTESIAN_POINT('Ctrl Pts',(1.82855629251586,1.65578252245344,-1.1308703926222));
#13638=CARTESIAN_POINT('Ctrl Pts',(1.83405019594872,1.65484848438915,-1.12190695532944));
#13639=CARTESIAN_POINT('Ctrl Pts',(1.84159744189999,1.65356535025961,-1.10959343969452));
#13640=CARTESIAN_POINT('Ctrl Pts',(1.84901495135613,1.65228221661491,-1.09720193972246));
#13641=CARTESIAN_POINT('Ctrl Pts',(1.85630043380627,1.65099908337441,-1.08473439120323));
#13642=CARTESIAN_POINT('Ctrl Pts',(1.94269536698868,1.63578304087669,-0.936887899410816));
#13643=CARTESIAN_POINT('Ctrl Pts',(2.01052212471306,1.62056705521867,-0.778350603268342));
#13644=CARTESIAN_POINT('Ctrl Pts',(2.05902851263356,1.60535099192654,-0.614115400509273));
#13645=CARTESIAN_POINT('Ctrl Pts',(2.08822076975288,1.59619361593938,-0.515274887485631));
#13646=CARTESIAN_POINT('Ctrl Pts',(2.11041582715717,1.58703621183384,-0.41436987553872));
#13647=CARTESIAN_POINT('Ctrl Pts',(2.12545410071187,1.57787875029803,-0.312480553990116));
#13648=CARTESIAN_POINT('Ctrl Pts',(2.14392857232465,1.56662883769515,-0.187309843951518));
#13649=CARTESIAN_POINT('Ctrl Pts',(2.1516346752806,1.55537901727325,-0.0604049918487018));
#13650=CARTESIAN_POINT('Ctrl Pts',(2.14816648894054,1.54412923482214,0.066174082986945));
#13651=CARTESIAN_POINT('Ctrl Pts',(2.14501081737324,1.53389315892013,0.181347245068504));
#13652=CARTESIAN_POINT('Ctrl Pts',(2.1326043268812,1.52365711445421,0.29624939231303));
#13653=CARTESIAN_POINT('Ctrl Pts',(2.11067724421865,1.51342106058787,0.409318422375977));
#13654=CARTESIAN_POINT('Ctrl Pts',(2.101743119398,1.50925041078825,0.455388063443951));
#13655=CARTESIAN_POINT('Ctrl Pts',(2.09122886378167,1.50507975942804,0.501153357089501));
#13656=CARTESIAN_POINT('Ctrl Pts',(2.07918943147896,1.50090910374499,0.546522634163261));
#13657=CARTESIAN_POINT('Ctrl Pts',(2.04903054684587,1.4904615742912,0.66017307537594));
#13658=CARTESIAN_POINT('Ctrl Pts',(2.00933880556038,1.48001401010943,0.771215375000161));
#13659=CARTESIAN_POINT('Ctrl Pts',(1.96098677543066,1.46956642993763,0.878354690721158));
#13660=CARTESIAN_POINT('Ctrl Pts',(1.91103606510354,1.45877341774391,0.989036391362615));
#13661=CARTESIAN_POINT('Ctrl Pts',(1.85184243190155,1.44798038848529,1.09555405084697));
#13662=CARTESIAN_POINT('Ctrl Pts',(1.78431417030651,1.43718736282047,1.19646961655335));
#13663=CARTESIAN_POINT('Ctrl Pts',(1.75668454824819,1.43277132703128,1.2377598685813));
#13664=CARTESIAN_POINT('Ctrl Pts',(1.72765906814075,1.42835529184374,1.27811204753106));
#13665=CARTESIAN_POINT('Ctrl Pts',(1.69729778749964,1.42393925867288,1.31742636891535));
#13666=CARTESIAN_POINT('Ctrl Pts',(1.63448216537924,1.41480275767311,1.3987652816308));
#13667=CARTESIAN_POINT('Ctrl Pts',(1.5658689249794,1.40566628773615,1.47575704033619));
#13668=CARTESIAN_POINT('Ctrl Pts',(1.49205385466478,1.39652983581773,1.54738069358613));
#13669=CARTESIAN_POINT('Ctrl Pts',(1.43633087498025,1.38963273035582,1.60144937303014));
#13670=CARTESIAN_POINT('Ctrl Pts',(1.3776446213347,1.3827356351622,1.65245912261462));
#13671=CARTESIAN_POINT('Ctrl Pts',(1.31626715210567,1.37583854462525,1.69998258358999));
#13672=CARTESIAN_POINT('Ctrl Pts',(1.23514282231084,1.36672246580394,1.76279568047367));
#13673=CARTESIAN_POINT('Ctrl Pts',(1.14931667202321,1.35760639511763,1.81951639687443));
#13674=CARTESIAN_POINT('Ctrl Pts',(1.05990936844222,1.34849031960903,1.869797824271));
#13675=CARTESIAN_POINT('Ctrl Pts',(1.05493841437683,1.34798347519258,1.87259341988702));
#13676=CARTESIAN_POINT('Ctrl Pts',(1.04995639555256,1.34747663076123,1.87536912224497));
#13677=CARTESIAN_POINT('Ctrl Pts',(1.04496350631085,1.34696978631274,1.87812487607801));
#13678=CARTESIAN_POINT('Ctrl Pts',(0.948041444385353,1.33713091213688,1.93161962245169));
#13679=CARTESIAN_POINT('Ctrl Pts',(0.847013429065949,1.32729195529011,1.97760765487141));
#13680=CARTESIAN_POINT('Ctrl Pts',(0.743106714900058,1.31745297843196,2.01575585739578));
#13681=CARTESIAN_POINT('Ctrl Pts',(0.638611050831489,1.30755823362359,2.05412028637235));
#13682=CARTESIAN_POINT('Ctrl Pts',(0.531202666028629,1.29766346857635,2.08455620521816));
#13683=CARTESIAN_POINT('Ctrl Pts',(0.422107829237246,1.2877687470214,2.10667806381857));
#13684=CARTESIAN_POINT('Ctrl Pts',(0.356803767358516,1.28184577644184,2.11992018659361));
#13685=CARTESIAN_POINT('Ctrl Pts',(0.290895084545275,1.27592282144646,2.13018228339791));
#13686=CARTESIAN_POINT('Ctrl Pts',(0.224644020099001,1.26999989570497,2.13737269833159));
#13687=CARTESIAN_POINT('Ctrl Pts',(0.123910472701584,1.26099419404722,2.14830559442287));
#13688=CARTESIAN_POINT('Ctrl Pts',(0.0223534651988909,1.25198849831628,
2.15213498225265));
#13689=CARTESIAN_POINT('Ctrl Pts',(-0.0789421896134073,1.24298279799778,
2.14852091627407));
#13690=CARTESIAN_POINT('Ctrl Pts',(-0.0967017060199631,1.24140388641607,
2.14788728530382));
#13691=CARTESIAN_POINT('Ctrl Pts',(-0.114453167950561,1.23982497469336,
2.14702498251185));
#13692=CARTESIAN_POINT('Ctrl Pts',(-0.132190712177884,1.23824606277296,
2.14593234183677));
#13693=CARTESIAN_POINT('Ctrl Pts',(-0.233511303782116,1.22922698505763,
2.13969094797804));
#13694=CARTESIAN_POINT('Ctrl Pts',(-0.334376984468477,1.22020790089213,
2.12592952298826));
#13695=CARTESIAN_POINT('Ctrl Pts',(-0.433744204604765,1.21118879971508,
2.10510452173353));
#13696=CARTESIAN_POINT('Ctrl Pts',(-0.500430189366313,1.20513602252326,
2.09112872856524));
#13697=CARTESIAN_POINT('Ctrl Pts',(-0.566441361409203,1.19908323766973,
2.07397276038877));
#13698=CARTESIAN_POINT('Ctrl Pts',(-0.631466910669559,1.19303044196224,
2.05378688774323));
#13699=CARTESIAN_POINT('Ctrl Pts',(-0.744235133770776,1.18253359842165,
2.01878026317985));
#13700=CARTESIAN_POINT('Ctrl Pts',(-0.854181326126747,1.17203672388374,
1.9746243355874));
#13701=CARTESIAN_POINT('Ctrl Pts',(-0.959890726345071,1.16153985212526,
1.92196464448792));
#13702=CARTESIAN_POINT('Ctrl Pts',(-1.06326499824549,1.15127485702525,1.87046820978422));
#13703=CARTESIAN_POINT('Ctrl Pts',(-1.16258876159359,1.14100986458324,1.81083883984471));
#13704=CARTESIAN_POINT('Ctrl Pts',(-1.25651370446884,1.13074490638656,1.7436387469327));
#13705=CARTESIAN_POINT('Ctrl Pts',(-1.30130124395243,1.12585012331342,1.71159479010437));
#13706=CARTESIAN_POINT('Ctrl Pts',(-1.34486071727869,1.12095534802699,1.67782885244961));
#13707=CARTESIAN_POINT('Ctrl Pts',(-1.38704268345722,1.11606058395213,1.64239916098616));
#13708=CARTESIAN_POINT('Ctrl Pts',(-1.43127877616563,1.110927460558,1.60524415712565));
#13709=CARTESIAN_POINT('Ctrl Pts',(-1.47398011128263,1.10579434261416,1.5662754013788));
#13710=CARTESIAN_POINT('Ctrl Pts',(-1.51496355146127,1.10066122536907,1.52557708359342));
#13711=CARTESIAN_POINT('Ctrl Pts',(-1.59936798859271,1.09008969038048,1.44175984936666));
#13712=CARTESIAN_POINT('Ctrl Pts',(-1.67648317419432,1.07951815835558,1.3506049926823));
#13713=CARTESIAN_POINT('Ctrl Pts',(-1.74557465267766,1.06894658778899,1.25371561483115));
#13714=CARTESIAN_POINT('Ctrl Pts',(-1.81061573468134,1.0589947615548,1.16250624851802));
#13715=CARTESIAN_POINT('Ctrl Pts',(-1.86854620040408,1.04904290116538,1.06621628618952));
#13716=CARTESIAN_POINT('Ctrl Pts',(-1.91879263515764,1.03909097199534,0.966198552429217));
#13717=CARTESIAN_POINT('Ctrl Pts',(-1.99132854275518,1.02472433646716,0.821812644658154));
#13718=CARTESIAN_POINT('Ctrl Pts',(-2.04803940956963,1.01035782592291,0.669303181233791));
#13719=CARTESIAN_POINT('Ctrl Pts',(-2.08711562508526,0.995991341057153,
0.512433188410289));
#13720=CARTESIAN_POINT('Ctrl Pts',(-2.11695159290074,0.985022060270358,
0.392657821340147));
#13721=CARTESIAN_POINT('Ctrl Pts',(-2.13650618310517,0.974052794453662,
0.27034060601716));
#13722=CARTESIAN_POINT('Ctrl Pts',(-2.14495718917906,0.96308349940367,0.147168803041655));
#13723=CARTESIAN_POINT('Ctrl Pts',(-2.14520431216876,0.962762737004021,
0.143567032562207));
#13724=CARTESIAN_POINT('Ctrl Pts',(-2.14544193953318,0.962441974579376,
0.139964532269499));
#13725=CARTESIAN_POINT('Ctrl Pts',(-2.14567008358036,0.962121212128629,
0.13636134679483));
#13726=CARTESIAN_POINT('Ctrl Pts',(-2.15516426399469,0.948772730697037,
-0.0135846780317181));
#13727=CARTESIAN_POINT('Ctrl Pts',(-2.14822099037921,0.935424286247537,
-0.164423349917931));
#13728=CARTESIAN_POINT('Ctrl Pts',(-2.12589474834246,0.922075809850497,
-0.312966252775792));
#13729=CARTESIAN_POINT('Ctrl Pts',(-2.10530864227326,0.90976773084108,-0.449931531080373));
#13730=CARTESIAN_POINT('Ctrl Pts',(-2.07164326047299,0.897459624670079,
-0.584946205874195));
#13731=CARTESIAN_POINT('Ctrl Pts',(-2.02569043015659,0.885151437301664,
-0.715528591157759));
#13732=CARTESIAN_POINT('Ctrl Pts',(-1.98749536130351,0.874921119370076,
-0.824066044945969));
#13733=CARTESIAN_POINT('Ctrl Pts',(-1.94073977799007,0.864690870679638,
-0.929727460777095));
#13734=CARTESIAN_POINT('Ctrl Pts',(-1.8858438432095,0.854460656230511,-1.03096115210299));
#13735=CARTESIAN_POINT('Ctrl Pts',(-1.83405290034749,0.844809077217991,
-1.126468922289));
#13736=CARTESIAN_POINT('Ctrl Pts',(-1.77501716663259,0.83515752868288,-1.21803465117041));
#13737=CARTESIAN_POINT('Ctrl Pts',(-1.70913035983726,0.825505981234695,
-1.30436705469545));
#13738=CARTESIAN_POINT('Ctrl Pts',(-1.6697089960266,0.819731271823253,-1.35602141849824));
#13739=CARTESIAN_POINT('Ctrl Pts',(-1.62783580702056,0.813956562800911,
-1.40580264114003));
#13740=CARTESIAN_POINT('Ctrl Pts',(-1.58375469431755,0.808181847872517,
-1.45355564552886));
#13741=CARTESIAN_POINT('Ctrl Pts',(-1.50663754512336,0.798079345340714,
-1.53709653953341));
#13742=CARTESIAN_POINT('Ctrl Pts',(-1.42282440888977,0.787976785588606,
-1.61437197301895));
#13743=CARTESIAN_POINT('Ctrl Pts',(-1.33353038165379,0.777874206994567,
-1.68469145621377));
#13744=CARTESIAN_POINT('Ctrl Pts',(-1.24208559852269,0.767528295434824,
-1.75670467019557));
#13745=CARTESIAN_POINT('Ctrl Pts',(-1.14489166109636,0.757182364114533,
-1.82142370215485));
#13746=CARTESIAN_POINT('Ctrl Pts',(-1.04321319294084,0.746836454252634,
-1.87807141801992));
#13747=CARTESIAN_POINT('Ctrl Pts',(-0.99202792284582,0.741628289729049,
-1.90658806160648));
#13748=CARTESIAN_POINT('Ctrl Pts',(-0.939705677254979,0.73642013064334,
-1.93305867581673));
#13749=CARTESIAN_POINT('Ctrl Pts',(-0.886405385013102,0.731211982253794,
-1.95737972730217));
#13750=CARTESIAN_POINT('Ctrl Pts',(-0.794655020321894,0.722246749719266,
-1.99924563928135));
#13751=CARTESIAN_POINT('Ctrl Pts',(-0.699914968864438,0.713281537187404,
-2.0347782125959));
#13752=CARTESIAN_POINT('Ctrl Pts',(-0.603126898273636,0.70431633524596,
-2.06336312897213));
#13753=CARTESIAN_POINT('Ctrl Pts',(-0.544120557004141,0.698850746748558,
-2.08078977381131));
#13754=CARTESIAN_POINT('Ctrl Pts',(-0.484353672977853,0.693385162187266,
-2.09563499587624));
#13755=CARTESIAN_POINT('Ctrl Pts',(-0.424043634817683,0.687919579429389,
-2.10776825003111));
#13756=CARTESIAN_POINT('Ctrl Pts',(-0.325219461550571,0.678963662405497,
-2.12764982940785));
#13757=CARTESIAN_POINT('Ctrl Pts',(-0.224937133287094,0.670007750223784,
-2.14024694311598));
#13758=CARTESIAN_POINT('Ctrl Pts',(-0.124301651299459,0.661051833501158,
-2.14573522960947));
#13759=CARTESIAN_POINT('Ctrl Pts',(-0.0987968483685675,0.6587820685379,
-2.14712616710666));
#13760=CARTESIAN_POINT('Ctrl Pts',(-0.0732693595882916,0.656512303282978,
-2.14806076265642));
#13761=CARTESIAN_POINT('Ctrl Pts',(-0.0477371270765782,0.65424253758365,
-2.14854240201057));
#13762=CARTESIAN_POINT('Ctrl Pts',(0.0636113333177027,0.644343876510439,
-2.15064287640213));
#13763=CARTESIAN_POINT('Ctrl Pts',(0.17510225252277,0.634445137226091,-2.14413424933341));
#13764=CARTESIAN_POINT('Ctrl Pts',(0.285465785627553,0.624546381844607,
-2.12925879840794));
#13765=CARTESIAN_POINT('Ctrl Pts',(0.395624804477018,0.614665969810136,
-2.11441091312561));
#13766=CARTESIAN_POINT('Ctrl Pts',(0.50466196196004,0.604785541738159,-2.09122694606622));
#13767=CARTESIAN_POINT('Ctrl Pts',(0.611310018100132,0.594905159398069,
-2.05989728951752));
#13768=CARTESIAN_POINT('Ctrl Pts',(0.674751543483836,0.589027635233859,
-2.04126027658795));
#13769=CARTESIAN_POINT('Ctrl Pts',(0.737347461353159,0.583150127252695,
-2.01973981883648));
#13770=CARTESIAN_POINT('Ctrl Pts',(0.798827280241264,0.577272648457316,
-1.99536799962312));
#13771=CARTESIAN_POINT('Ctrl Pts',(0.892778217051504,0.568290926505382,
-1.95812398543641));
#13772=CARTESIAN_POINT('Ctrl Pts',(0.984119740890388,0.559309210317195,
-1.9142168626982));
#13773=CARTESIAN_POINT('Ctrl Pts',(1.07174864050312,0.550327485872927,-1.86382801026776));
#13774=CARTESIAN_POINT('Ctrl Pts',(1.16191422281691,0.541085758334656,-1.81198050058097));
#13775=CARTESIAN_POINT('Ctrl Pts',(1.24814793734788,0.531844022055364,-1.75327086036017));
#13776=CARTESIAN_POINT('Ctrl Pts',(1.3296681927492,0.522602261762046,-1.68863020361191));
#13777=CARTESIAN_POINT('Ctrl Pts',(1.39523376777737,0.515169246189157,-1.63664064826724));
#13778=CARTESIAN_POINT('Ctrl Pts',(1.45775066054175,0.507736215082205,-1.58081561857954));
#13779=CARTESIAN_POINT('Ctrl Pts',(1.51683029451761,0.500303160495069,-1.52165601801066));
#13780=CARTESIAN_POINT('Ctrl Pts',(1.6046859462726,0.489249675371074,-1.43368145019824));
#13781=CARTESIAN_POINT('Ctrl Pts',(1.68508261411045,0.478196192393638,-1.338202241932));
#13782=CARTESIAN_POINT('Ctrl Pts',(1.75685157244071,0.467142721989082,-1.23663042913025));
#13783=CARTESIAN_POINT('Ctrl Pts',(1.82625242210846,0.456453974991759,-1.13841010832946));
#13784=CARTESIAN_POINT('Ctrl Pts',(1.88758618313705,0.445765239751282,-1.03449142167311));
#13785=CARTESIAN_POINT('Ctrl Pts',(1.93975294714389,0.435076525695469,-0.926130709139889));
#13786=CARTESIAN_POINT('Ctrl Pts',(1.95885737315287,0.431162122517544,-0.886447028269824));
#13787=CARTESIAN_POINT('Ctrl Pts',(1.97673188425863,0.42724772218082,-0.846167484490858));
#13788=CARTESIAN_POINT('Ctrl Pts',(1.99332068309008,0.423333325148358,-0.805353531339599));
#13789=CARTESIAN_POINT('Ctrl Pts',(2.00827610756237,0.419804349375709,-0.768558221445805));
#13790=CARTESIAN_POINT('Ctrl Pts',(2.0221803966365,0.416275377002179,-0.731343412060049));
#13791=CARTESIAN_POINT('Ctrl Pts',(2.03499339342307,0.412746406294115,-0.693759244140605));
#13792=CARTESIAN_POINT('Ctrl Pts',(2.07801870352698,0.400896324569193,-0.567553758674014));
#13793=CARTESIAN_POINT('Ctrl Pts',(2.10873496467875,0.38904626162368,-0.437183446883494));
#13794=CARTESIAN_POINT('Ctrl Pts',(2.12723591878782,0.377196151815658,-0.305089849806085));
#13795=CARTESIAN_POINT('Ctrl Pts',(2.14328155922495,0.366918703420348,-0.190526765639993));
#13796=CARTESIAN_POINT('Ctrl Pts',(2.1501398316329,0.35664121977568,-0.0746682717553836));
#13797=CARTESIAN_POINT('Ctrl Pts',(2.14790281915223,0.346363658059301,0.0409003818768428));
#13798=CARTESIAN_POINT('Ctrl Pts',(2.14479530958078,0.332086750048781,0.201440700907735));
#13799=CARTESIAN_POINT('Ctrl Pts',(2.12413003425264,0.317809987717386,0.361830411071172));
#13800=CARTESIAN_POINT('Ctrl Pts',(2.0859467663204,0.303533255949083,0.517891861201881));
#13801=CARTESIAN_POINT('Ctrl Pts',(2.06065926664616,0.294078254596637,0.62124613345392));
#13802=CARTESIAN_POINT('Ctrl Pts',(2.02768927911112,0.284623266649076,0.72270102301507));
#13803=CARTESIAN_POINT('Ctrl Pts',(1.98705824020302,0.275168258668891,0.82103565699802));
#13804=CARTESIAN_POINT('Ctrl Pts',(1.97878691214473,0.273243486994341,0.841053801722414));
#13805=CARTESIAN_POINT('Ctrl Pts',(1.97019812461692,0.271318714489611,0.860942626125018));
#13806=CARTESIAN_POINT('Ctrl Pts',(1.96129871595332,0.269393940872609,0.880694548915241));
#13807=CARTESIAN_POINT('Ctrl Pts',(1.90856578436955,0.257988806071383,0.99773342559981));
#13808=CARTESIAN_POINT('Ctrl Pts',(1.84501274575367,0.246583674668671,1.10978491333392));
#13809=CARTESIAN_POINT('Ctrl Pts',(1.77210366778145,0.235178527568502,1.21539096611084));
#13810=CARTESIAN_POINT('Ctrl Pts',(1.69551977918379,0.223198530848588,1.32631984363946));
#13811=CARTESIAN_POINT('Ctrl Pts',(1.60861231781684,0.211218516808914,1.43013841101961));
#13812=CARTESIAN_POINT('Ctrl Pts',(1.51302369362006,0.199238463318028,1.52514280501988));
#13813=CARTESIAN_POINT('Ctrl Pts',(1.494899900635,0.196967021383977,1.54315582679942));
#13814=CARTESIAN_POINT('Ctrl Pts',(1.47646389638305,0.194695578031699,1.56085191741852));
#13815=CARTESIAN_POINT('Ctrl Pts',(1.45772670097547,0.192424133110347,1.57821935062689));
#13816=CARTESIAN_POINT('Ctrl Pts',(1.37836677344921,0.182803605575825,1.6517777573549));
#13817=CARTESIAN_POINT('Ctrl Pts',(1.29348115512078,0.173183129264224,1.71954821041346));
#13818=CARTESIAN_POINT('Ctrl Pts',(1.20397049377609,0.163562681136566,1.7805144196128));
#13819=CARTESIAN_POINT('Ctrl Pts',(1.12341823457021,0.154905066282492,1.83537901129886));
#13820=CARTESIAN_POINT('Ctrl Pts',(1.03912148844003,0.14624747425328,1.8847329446552));
#13821=CARTESIAN_POINT('Ctrl Pts',(0.951761962758758,0.137589888258096,
1.92786129340198));
#13822=CARTESIAN_POINT('Ctrl Pts',(0.877309773645605,0.130211457288489,
1.96461744508656));
#13823=CARTESIAN_POINT('Ctrl Pts',(0.800633647658955,0.122833030701572,
1.9968521186444));
#13824=CARTESIAN_POINT('Ctrl Pts',(0.722342758034967,0.115454598103574,
2.02450263203523));
#13825=CARTESIAN_POINT('Ctrl Pts',(0.617134365294067,0.105539357156503,
2.06165977875155));
#13826=CARTESIAN_POINT('Ctrl Pts',(0.509052265328476,0.0956240427058641,
2.09053133521612));
#13827=CARTESIAN_POINT('Ctrl Pts',(0.399404995198041,0.0857087073856261,
2.11104089390714));
#13828=CARTESIAN_POINT('Ctrl Pts',(0.287985874873716,0.0756331447401773,
2.1318818777718));
#13829=CARTESIAN_POINT('Ctrl Pts',(0.174949242882979,0.0655575605451831,
2.14408869178551));
#13830=CARTESIAN_POINT('Ctrl Pts',(0.0616511258305347,0.0554820100277887,
2.14753105216021));
#13831=CARTESIAN_POINT('Ctrl Pts',(-0.00205973434369371,0.0498162319293323,
2.14946679254326));
#13832=CARTESIAN_POINT('Ctrl Pts',(-0.0658534701497418,0.0441504644802167,
2.14863016618283));
#13833=CARTESIAN_POINT('Ctrl Pts',(-0.12948877016016,0.0384847175007255,
2.14499074027714));
#13834=CARTESIAN_POINT('Ctrl Pts',(-0.229535572857717,0.0295770849430313,
2.13926887009724));
#13835=CARTESIAN_POINT('Ctrl Pts',(-0.32926218534485,0.0206694642280899,
2.12660962764732));
#13836=CARTESIAN_POINT('Ctrl Pts',(-0.427570331839619,0.0117618471326195,
2.10688913349251));
#13837=CARTESIAN_POINT('Ctrl Pts',(-0.470839874821073,0.00784123084071015,
2.09820931600158));
#13838=CARTESIAN_POINT('Ctrl Pts',(-0.513834571500548,0.00392061524998314,
2.08816222949006));
#13839=CARTESIAN_POINT('Ctrl Pts',(-0.556460950674994,-3.40744243931823E-10,
2.07674052552866));
#13840=CARTESIAN_POINT('Ctrl Pts',(-0.653307832806579,-0.00890761584438663,
2.05079048147811));
#13841=CARTESIAN_POINT('Ctrl Pts',(-0.748251944292738,-0.0178152313480485,
2.01774148912384));
#13842=CARTESIAN_POINT('Ctrl Pts',(-0.840392897999384,-0.0267228550750663,
1.97822993810398));
#13843=CARTESIAN_POINT('Ctrl Pts',(-0.880947998121618,-0.0306434740568333,
1.96083924652619));
#13844=CARTESIAN_POINT('Ctrl Pts',(-0.920960336094546,-0.0345640946316652,
1.94219722621708));
#13845=CARTESIAN_POINT('Ctrl Pts',(-0.960354805675053,-0.0384847175007351,
1.92236085704252));
#13846=CARTESIAN_POINT('Ctrl Pts',(-1.06141534381935,-0.0485424809692676,
1.871473659805));
#13847=CARTESIAN_POINT('Ctrl Pts',(-1.1584932522127,-0.0586003089435517,
1.8126904579763));
#13848=CARTESIAN_POINT('Ctrl Pts',(-1.25050001533805,-0.0686581464875737,
1.74682307061668));
#13849=CARTESIAN_POINT('Ctrl Pts',(-1.34161250164382,-0.0786182250118753,
1.68159589355988));
#13850=CARTESIAN_POINT('Ctrl Pts',(-1.42775300990498,-0.0885783129207585,
1.60942070905301));
#13851=CARTESIAN_POINT('Ctrl Pts',(-1.50783543107933,-0.0985383568645636,
1.53104539645999));
#13852=CARTESIAN_POINT('Ctrl Pts',(-1.55317317335856,-0.104177121262445,
1.48667411408254));
#13853=CARTESIAN_POINT('Ctrl Pts',(-1.59656860554779,-0.109815871568963,
1.4403149458517));
#13854=CARTESIAN_POINT('Ctrl Pts',(-1.6378184947156,-0.115454598103576,
1.39209933035345));
#13855=CARTESIAN_POINT('Ctrl Pts',(-1.69179513731939,-0.122833030701568,
1.32900783851737));
#13856=CARTESIAN_POINT('Ctrl Pts',(-1.74208127350863,-0.130211457288479,
1.26275372934031));
#13857=CARTESIAN_POINT('Ctrl Pts',(-1.78818068480565,-0.13758988825808,
1.1936958736796));
#13858=CARTESIAN_POINT('Ctrl Pts',(-1.84828770736962,-0.147210304317604,
1.10365433146394));
#13859=CARTESIAN_POINT('Ctrl Pts',(-1.90127508606266,-0.156830727827904,
1.00884599998052));
#13860=CARTESIAN_POINT('Ctrl Pts',(-1.94682567081003,-0.166451181827962,
0.910589167921595));
#13861=CARTESIAN_POINT('Ctrl Pts',(-1.98781746390209,-0.175108801966302,
0.822166071884982));
#13862=CARTESIAN_POINT('Ctrl Pts',(-2.02278698960568,-0.183766446796818,
0.730951298313189));
#13863=CARTESIAN_POINT('Ctrl Pts',(-2.05153803013303,-0.192424133110348,
0.637914699899324));
#13864=CARTESIAN_POINT('Ctrl Pts',(-2.09139068444731,-0.20442480416385,
0.508953962230096));
#13865=CARTESIAN_POINT('Ctrl Pts',(-2.11937975563295,-0.216425431419754,
0.376252287616784));
#13866=CARTESIAN_POINT('Ctrl Pts',(-2.13494174468323,-0.228426037123835,
0.242118082797647));
#13867=CARTESIAN_POINT('Ctrl Pts',(-2.1497621600032,-0.2398547793014,0.114375760295607));
#13868=CARTESIAN_POINT('Ctrl Pts',(-2.1533115885628,-0.251283501932252,
-0.0146671125818596));
#13869=CARTESIAN_POINT('Ctrl Pts',(-2.14505715479067,-0.26271222423113,
-0.14300745196953));
#13870=CARTESIAN_POINT('Ctrl Pts',(-2.14344852391613,-0.264939463076827,
-0.168018523363072));
#13871=CARTESIAN_POINT('Ctrl Pts',(-2.14139145421298,-0.267166701909915,
-0.193002851471323));
#13872=CARTESIAN_POINT('Ctrl Pts',(-2.13888178688306,-0.269393940872609,
-0.217945505641568));
#13873=CARTESIAN_POINT('Ctrl Pts',(-2.13671293946929,-0.271318714489607,
-0.239500876883247));
#13874=CARTESIAN_POINT('Ctrl Pts',(-2.13420663545479,-0.273243486994335,
-0.261019497831176));
#13875=CARTESIAN_POINT('Ctrl Pts',(-2.13136074331412,-0.275168258668881,
-0.28249138372823));
#13876=CARTESIAN_POINT('Ctrl Pts',(-2.1102517111346,-0.289445000445393,
-0.441756284838774));
#13877=CARTESIAN_POINT('Ctrl Pts',(-2.07045749324644,-0.303721696547568,
-0.598446701518509));
#13878=CARTESIAN_POINT('Ctrl Pts',(-2.01401963788178,-0.317998462091363,
-0.748892742727702));
#13879=CARTESIAN_POINT('Ctrl Pts',(-1.97664273626235,-0.327453485811278,
-0.848528117689688));
#13880=CARTESIAN_POINT('Ctrl Pts',(-1.93196655588015,-0.336908539988082,
-0.945425405945982));
#13881=CARTESIAN_POINT('Ctrl Pts',(-1.88058859718454,-0.346363658059302,
-1.03853063984612));
#13882=CARTESIAN_POINT('Ctrl Pts',(-1.81619583542424,-0.358213898528815,
-1.15522081784032));
#13883=CARTESIAN_POINT('Ctrl Pts',(-1.74113749645292,-0.370064035205387,
-1.26619866219996));
#13884=CARTESIAN_POINT('Ctrl Pts',(-1.65650994003969,-0.381914133730994,
-1.369289610165));
#13885=CARTESIAN_POINT('Ctrl Pts',(-1.58311354473584,-0.392191572341276,
-1.45869906838148));
#13886=CARTESIAN_POINT('Ctrl Pts',(-1.50252055125346,-0.402468982254876,
-1.54217545295685));
#13887=CARTESIAN_POINT('Ctrl Pts',(-1.41547635316767,-0.412746406294107,
-1.61830982624727));
#13888=CARTESIAN_POINT('Ctrl Pts',(-1.38558788849214,-0.416275377002174,
-1.64445217205234));
#13889=CARTESIAN_POINT('Ctrl Pts',(-1.35493901623949,-0.419804349375706,
-1.66972899784035));
#13890=CARTESIAN_POINT('Ctrl Pts',(-1.32358958377519,-0.423333325148358,
-1.69411695871237));
#13891=CARTESIAN_POINT('Ctrl Pts',(-1.22901514748013,-0.433979479421723,
-1.76769014554705));
#13892=CARTESIAN_POINT('Ctrl Pts',(-1.12818410298468,-0.444625658136703,
-1.83308698183334));
#13893=CARTESIAN_POINT('Ctrl Pts',(-1.02267279851515,-0.455271851977543,
-1.88978810786402));
#13894=CARTESIAN_POINT('Ctrl Pts',(-0.913233663837565,-0.466314367728904,
-1.94860002568875));
#13895=CARTESIAN_POINT('Ctrl Pts',(-0.798758150774989,-0.477356899753293,
-1.99805751311023));
#13896=CARTESIAN_POINT('Ctrl Pts',(-0.680967747542164,-0.48839943765537,
-2.03754066959344));
#13897=CARTESIAN_POINT('Ctrl Pts',(-0.638642208663121,-0.492367344670458,
-2.05172812314595));
#13898=CARTESIAN_POINT('Ctrl Pts',(-0.595888406433419,-0.496335252444458,
-2.06462729201675));
#13899=CARTESIAN_POINT('Ctrl Pts',(-0.552785559276754,-0.500303160495067,
-2.07620791467739));
#13900=CARTESIAN_POINT('Ctrl Pts',(-0.452393043337931,-0.50954496929639,
-2.10318079284514));
#13901=CARTESIAN_POINT('Ctrl Pts',(-0.349975592528666,-0.518786741799876,
-2.12303119653041));
#13902=CARTESIAN_POINT('Ctrl Pts',(-0.24666352700019,-0.528028493278499,
-2.13530341028129));
#13903=CARTESIAN_POINT('Ctrl Pts',(-0.163571110884956,-0.535461501761749,
-2.14517377621025));
#13904=CARTESIAN_POINT('Ctrl Pts',(-0.0799008481762825,-0.542894496644514,
-2.15014272792901));
#13905=CARTESIAN_POINT('Ctrl Pts',(0.00375245598683078,-0.550327485872929,
-2.14999672542845));
#13906=CARTESIAN_POINT('Ctrl Pts',(0.104835735372361,-0.559309210317197,
-2.14982030189441));
#13907=CARTESIAN_POINT('Ctrl Pts',(0.205893376806318,-0.568290926505382,
-2.14217422367334));
#13908=CARTESIAN_POINT('Ctrl Pts',(0.305879281886703,-0.577272648457315,
-2.12745301769284));
#13909=CARTESIAN_POINT('Ctrl Pts',(0.415433915962271,-0.587113928195907,
-2.11132298083365));
#13910=CARTESIAN_POINT('Ctrl Pts',(0.523701381992398,-0.596955289760699,
-2.08670807798976));
#13911=CARTESIAN_POINT('Ctrl Pts',(0.629506698707356,-0.606796672111442,
-2.05410204499644));
#13912=CARTESIAN_POINT('Ctrl Pts',(0.7362266343023,-0.616723126879929,-2.02121415382905));
#13913=CARTESIAN_POINT('Ctrl Pts',(0.840442973658776,-0.626649602795276,
-1.98019595821689));
#13914=CARTESIAN_POINT('Ctrl Pts',(0.940939887621261,-0.636576037220439,
-1.93150309431318));
#13915=CARTESIAN_POINT('Ctrl Pts',(1.00055963316546,-0.642464889636447,
-1.90261607638105));
#13916=CARTESIAN_POINT('Ctrl Pts',(1.0588700592828,-0.648353727450196,-1.87102705996308));
#13917=CARTESIAN_POINT('Ctrl Pts',(1.11561276575759,-0.654242537583649,
-1.83682373771093));
#13918=CARTESIAN_POINT('Ctrl Pts',(1.20190916640318,-0.663198457210571,
-1.7848060638308));
#13919=CARTESIAN_POINT('Ctrl Pts',(1.28461395722914,-0.672154369918574,
-1.72671438540263));
#13920=CARTESIAN_POINT('Ctrl Pts',(1.36267612235558,-0.681110285090713,
-1.66293744887761));
#13921=CARTESIAN_POINT('Ctrl Pts',(1.38246000075157,-0.683380049661083,
-1.64677398281648));
#13922=CARTESIAN_POINT('Ctrl Pts',(1.40194579851717,-0.685649814389728,
-1.63024558168205));
#13923=CARTESIAN_POINT('Ctrl Pts',(1.42111668508107,-0.687919579429389,
-1.61335903240838));
#13924=CARTESIAN_POINT('Ctrl Pts',(1.49683848269127,-0.696884771956248,
-1.54665998527912));
#13925=CARTESIAN_POINT('Ctrl Pts',(1.56764415040306,-0.705849969335355,
-1.47437066573726));
#13926=CARTESIAN_POINT('Ctrl Pts',(1.63299881687974,-0.714815180979017,
-1.39747640935412));
#13927=CARTESIAN_POINT('Ctrl Pts',(1.67284194765184,-0.7202807753914,-1.35059822791942));
#13928=CARTESIAN_POINT('Ctrl Pts',(1.71065986859473,-0.725746375105432,
-1.30200929725504));
#13929=CARTESIAN_POINT('Ctrl Pts',(1.74633944512399,-0.731211982253794,
-1.25193787618981));
#13930=CARTESIAN_POINT('Ctrl Pts',(1.81383563057361,-0.741551444477461,
-1.1572161824171));
#13931=CARTESIAN_POINT('Ctrl Pts',(1.87376027274665,-0.751890948856925,
-1.05708688572005));
#13932=CARTESIAN_POINT('Ctrl Pts',(1.92543098634018,-0.762230454249894,
-0.952865578606035));
#13933=CARTESIAN_POINT('Ctrl Pts',(1.97615540761795,-0.772380602968229,
-0.850552970157105));
#13934=CARTESIAN_POINT('Ctrl Pts',(2.01892596431358,-0.782530752663265,
-0.744295584274527));
#13935=CARTESIAN_POINT('Ctrl Pts',(2.05305207438863,-0.792680864412052,
-0.635318870181491));
#13936=CARTESIAN_POINT('Ctrl Pts',(2.07042427884942,-0.797847870443853,
-0.57984328991393));
#13937=CARTESIAN_POINT('Ctrl Pts',(2.08555557901215,-0.803014866642226,
-0.523662827821059));
#13938=CARTESIAN_POINT('Ctrl Pts',(2.09834962140627,-0.808181847872517,
-0.466938767683641));
#13939=CARTESIAN_POINT('Ctrl Pts',(2.11264848263973,-0.81395656280091,-0.403542896424378));
#13940=CARTESIAN_POINT('Ctrl Pts',(2.12402111673552,-0.81973127182325,-0.339494498482121));
#13941=CARTESIAN_POINT('Ctrl Pts',(2.13233383734598,-0.825505981234692,
-0.275049825307238));
#13942=CARTESIAN_POINT('Ctrl Pts',(2.14706022967544,-0.835736162226755,
-0.160882925541307));
#13943=CARTESIAN_POINT('Ctrl Pts',(2.15218037387138,-0.845966344439981,
-0.0454727405449347));
#13944=CARTESIAN_POINT('Ctrl Pts',(2.14805857657556,-0.856196562874184,
0.0696147130120628));
#13945=CARTESIAN_POINT('Ctrl Pts',(2.14416991397958,-0.8658481456471,0.178192656999639));
#13946=CARTESIAN_POINT('Ctrl Pts',(2.1320559120424,-0.875499760659425,0.286482292885839));
#13947=CARTESIAN_POINT('Ctrl Pts',(2.11206366829738,-0.885151437301663,
0.393179278001693));
#13948=CARTESIAN_POINT('Ctrl Pts',(2.08441372175388,-0.898500031217214,
0.5407448025337));
#13949=CARTESIAN_POINT('Ctrl Pts',(2.04164123141159,-0.911848529627996,
0.685599334388376));
#13950=CARTESIAN_POINT('Ctrl Pts',(1.98445313399436,-0.925197001463674,
0.824494840372859));
#13951=CARTESIAN_POINT('Ctrl Pts',(1.93172235030964,-0.937505076267311,
0.952564652302691));
#13952=CARTESIAN_POINT('Ctrl Pts',(1.866734999188,-0.949813128477027,1.0755686879077));
#13953=CARTESIAN_POINT('Ctrl Pts',(1.79002412712317,-0.962121212128629,
1.19092743220905));
#13954=CARTESIAN_POINT('Ctrl Pts',(1.78802495584534,-0.962441974579362,
1.19393381034094));
#13955=CARTESIAN_POINT('Ctrl Pts',(1.78601791436486,-0.962762737003993,
1.19693485342922));
#13956=CARTESIAN_POINT('Ctrl Pts',(1.78400301433828,-0.963083499403627,
1.19993051666803));
#13957=CARTESIAN_POINT('Ctrl Pts',(1.69375843327332,-0.977450002949473,
1.33410212341423));
#13958=CARTESIAN_POINT('Ctrl Pts',(1.58775427402266,-0.991816456350905,
1.45748085014487));
#13959=CARTESIAN_POINT('Ctrl Pts',(1.46947880964235,-1.0061829589133,1.56770856745458));
#13960=CARTESIAN_POINT('Ctrl Pts',(1.37917162655664,-1.01715225321286,1.65187103259783));
#13961=CARTESIAN_POINT('Ctrl Pts',(1.28170911994277,-1.0281215761724,1.72836702686252));
#13962=CARTESIAN_POINT('Ctrl Pts',(1.17862389042603,-1.03909097199534,1.79614880908248));
#13963=CARTESIAN_POINT('Ctrl Pts',(1.07927620822019,-1.04966265190832,1.86147303633505));
#13964=CARTESIAN_POINT('Ctrl Pts',(0.974522219696174,-1.0602342542074,1.91881853880723));
#13965=CARTESIAN_POINT('Ctrl Pts',(0.865769157978579,-1.070805820398,1.96712566934777));
#13966=CARTESIAN_POINT('Ctrl Pts',(0.763391600568948,-1.0807576425122,2.0126008582951));
#13967=CARTESIAN_POINT('Ctrl Pts',(0.657471367298694,-1.09070943262743,
2.05006596767214));
#13968=CARTESIAN_POINT('Ctrl Pts',(0.549208379576276,-1.10066122536905,
2.07867028555393));
#13969=CARTESIAN_POINT('Ctrl Pts',(0.493366520354362,-1.10579434261414,
2.09342434255806));
#13970=CARTESIAN_POINT('Ctrl Pts',(0.436901701494061,-1.11092746055799,
2.10582160743021));
#13971=CARTESIAN_POINT('Ctrl Pts',(0.380014619514122,-1.11606058395213,
2.11588073829693));
#13972=CARTESIAN_POINT('Ctrl Pts',(0.266781811981912,-1.12627798222775,
2.13590327398919));
#13973=CARTESIAN_POINT('Ctrl Pts',(0.151977035804607,-1.13649542935549,
2.14664964747342));
#13974=CARTESIAN_POINT('Ctrl Pts',(0.0370366125123074,-1.14671289418464,
2.14832797671703));
#13975=CARTESIAN_POINT('Ctrl Pts',(-0.0810644601923213,-1.15721132043087,
2.15005245691595));
#13976=CARTESIAN_POINT('Ctrl Pts',(-0.199310124060812,-1.16770976536543,
2.14220340823848));
#13977=CARTESIAN_POINT('Ctrl Pts',(-0.316153836373017,-1.17820819519649,
2.12495366561866));
#13978=CARTESIAN_POINT('Ctrl Pts',(-0.371142628313499,-1.18314894863763,
2.11683562067489));
#13979=CARTESIAN_POINT('Ctrl Pts',(-0.425820945600476,-1.18808969873363,
2.10663473889586));
#13980=CARTESIAN_POINT('Ctrl Pts',(-0.480027057582445,-1.19303044196224,
2.09436507407996));
#13981=CARTESIAN_POINT('Ctrl Pts',(-0.578978142735444,-1.20204957072943,
2.07196729265631));
#13982=CARTESIAN_POINT('Ctrl Pts',(-0.676460590337036,-1.2110686753973,
2.04264685296404));
#13983=CARTESIAN_POINT('Ctrl Pts',(-0.771335842863926,-1.2200877665272,
2.00649586702304));
#13984=CARTESIAN_POINT('Ctrl Pts',(-0.83500723907403,-1.22614053697568,
1.98223470631011));
#13985=CARTESIAN_POINT('Ctrl Pts',(-0.897504289009474,-1.23219330132686,
1.95489826292322));
#13986=CARTESIAN_POINT('Ctrl Pts',(-0.958485656028116,-1.23824606277299,
1.92452727892239));
#13987=CARTESIAN_POINT('Ctrl Pts',(-1.04921780185708,-1.2472517650235,1.87933930292163));
#13988=CARTESIAN_POINT('Ctrl Pts',(-1.13659283713798,-1.25625746084299,
1.82743191255314));
#13989=CARTESIAN_POINT('Ctrl Pts',(-1.21983547650336,-1.2652631607459,1.76963483802778));
#13990=CARTESIAN_POINT('Ctrl Pts',(-1.23442987368726,-1.26684207225452,
1.75950164825724));
#13991=CARTESIAN_POINT('Ctrl Pts',(-1.24889732962621,-1.26842098388866,
1.74918751959763));
#13992=CARTESIAN_POINT('Ctrl Pts',(-1.2632337773796,-1.26999989570497,1.73869704406139));
#13993=CARTESIAN_POINT('Ctrl Pts',(-1.35279273421466,-1.27986326616023,
1.67316365239487));
#13994=CARTESIAN_POINT('Ctrl Pts',(-1.43727166003755,-1.28972671774178,
1.60073036213476));
#13995=CARTESIAN_POINT('Ctrl Pts',(-1.51582812240706,-1.29959018732102,
1.52236007107001));
#13996=CARTESIAN_POINT('Ctrl Pts',(-1.59447737559033,-1.30946530762054,
1.44389720909685));
#13997=CARTESIAN_POINT('Ctrl Pts',(-1.66719110375498,-1.31934044596026,
1.35948231302115));
#13998=CARTESIAN_POINT('Ctrl Pts',(-1.73309015729065,-1.32921553898753,
1.27004330919134));
#13999=CARTESIAN_POINT('Ctrl Pts',(-1.7725831932114,-1.33513364224883,1.21644287638613));
#14000=CARTESIAN_POINT('Ctrl Pts',(-1.8096279889798,-1.34105172923591,1.16103734046149));
#14001=CARTESIAN_POINT('Ctrl Pts',(-1.84402738053199,-1.34696978631274,
1.10402210100787));
#14002=CARTESIAN_POINT('Ctrl Pts',(-1.89701562762061,-1.35608586239785,
1.01619678027794));
#14003=CARTESIAN_POINT('Ctrl Pts',(-1.94372842826759,-1.36520193294027,
0.924538465851365));
#14004=CARTESIAN_POINT('Ctrl Pts',(-1.983366316552,-1.37431801089728,0.82990628909204));
#14005=CARTESIAN_POINT('Ctrl Pts',(-1.98557014234611,-1.37482485544961,
0.824644837457733));
#14006=CARTESIAN_POINT('Ctrl Pts',(-1.98775210914776,-1.37533170002485,
0.819374200175097));
#14007=CARTESIAN_POINT('Ctrl Pts',(-1.98991208368564,-1.37583854462525,
0.814094527327367));
#14008=CARTESIAN_POINT('Ctrl Pts',(-2.02884800367239,-1.38497497677321,
0.71892260934876));
#14009=CARTESIAN_POINT('Ctrl Pts',(-2.06063345853673,-1.39411141709258,
0.620813452405457));
#14010=CARTESIAN_POINT('Ctrl Pts',(-2.08522380920602,-1.40324787862765,
0.520945067607857));
#14011=CARTESIAN_POINT('Ctrl Pts',(-2.10378705929605,-1.4101449913486,0.445554446790037));
#14012=CARTESIAN_POINT('Ctrl Pts',(-2.11825105895416,-1.4170421161598,0.369161879812258));
#14013=CARTESIAN_POINT('Ctrl Pts',(-2.12861618621955,-1.42393925867289,
0.292275809346556));
#14014=CARTESIAN_POINT('Ctrl Pts',(-2.14484500772538,-1.43473820902624,
0.171894237376967));
#14015=CARTESIAN_POINT('Ctrl Pts',(-2.15105642268712,-1.4455371714393,0.0501320965044703));
#14016=CARTESIAN_POINT('Ctrl Pts',(-2.14720407173045,-1.45633612521925,
-0.0713091123552385));
#14017=CARTESIAN_POINT('Ctrl Pts',(-2.14346081128115,-1.46682927525492,
-0.189311360632586));
#14018=CARTESIAN_POINT('Ctrl Pts',(-2.13021549798078,-1.47732241713949,
-0.307011950828631));
#14019=CARTESIAN_POINT('Ctrl Pts',(-2.10737820057378,-1.48781553188887,
-0.422842016555831));
#14020=CARTESIAN_POINT('Ctrl Pts',(-2.09787920513487,-1.49218006099089,
-0.47102062746686));
#14021=CARTESIAN_POINT('Ctrl Pts',(-2.08672015986324,-1.49654458539831,
-0.518875413538272));
#14022=CARTESIAN_POINT('Ctrl Pts',(-2.07389218402246,-1.50090910374499,
-0.566292230810799));
#14023=CARTESIAN_POINT('Ctrl Pts',(-2.06163399970687,-1.50507975942804,
-0.611602893459367));
#14024=CARTESIAN_POINT('Ctrl Pts',(-2.04785696534972,-1.50925041078825,
-0.656493928176217));
#14025=CARTESIAN_POINT('Ctrl Pts',(-2.03255932387099,-1.51342106058787,
-0.700858470094616));
#14026=CARTESIAN_POINT('Ctrl Pts',(-1.99129602523472,-1.52467081882205,
-0.820525762898292));
#14027=CARTESIAN_POINT('Ctrl Pts',(-1.9389660390348,-1.53592056570171,-0.936360310291058));
#14028=CARTESIAN_POINT('Ctrl Pts',(-1.87691822783045,-1.547170355437,-1.04674670439718));
#14029=CARTESIAN_POINT('Ctrl Pts',(-1.82046148231699,-1.55740643796493,
-1.14718629185777));
#14030=CARTESIAN_POINT('Ctrl Pts',(-1.75596049599052,-1.56764255597309,
-1.24311491750237));
#14031=CARTESIAN_POINT('Ctrl Pts',(-1.68445696879917,-1.57787875029803,
-1.33334314829979));
#14032=CARTESIAN_POINT('Ctrl Pts',(-1.57816625909843,-1.5930949557381,-1.46746831754962));
#14033=CARTESIAN_POINT('Ctrl Pts',(-1.45611949820129,-1.60831100261461,
-1.58936165575153));
#14034=CARTESIAN_POINT('Ctrl Pts',(-1.32143778516597,-1.6235270254014,-1.69509164555733));
#14035=CARTESIAN_POINT('Ctrl Pts',(-1.2403832402782,-1.63268437701351,-1.75872237917036));
#14036=CARTESIAN_POINT('Ctrl Pts',(-1.1547533596122,-1.64184171990055,-1.81649828441596));
#14037=CARTESIAN_POINT('Ctrl Pts',(-1.06523613713058,-1.6509990833744,-1.86755775604367));
#14038=CARTESIAN_POINT('Ctrl Pts',(-1.05269294999024,-1.65228221661491,
-1.87471222855922));
#14039=CARTESIAN_POINT('Ctrl Pts',(-1.0400734483823,-1.65356535025962,-1.881734827598));
#14040=CARTESIAN_POINT('Ctrl Pts',(-1.02738058384234,-1.65484848438917,
-1.88862502197215));
#14041=CARTESIAN_POINT('Ctrl Pts',(-0.909721814516881,-1.66674272481745,
-1.95249490634092));
#14042=CARTESIAN_POINT('Ctrl Pts',(-0.785960307043669,-1.67863694886956,
-2.00488317907329));
#14043=CARTESIAN_POINT('Ctrl Pts',(-0.658433952223786,-1.6905311913999,
-2.04549523452568));
#14044=CARTESIAN_POINT('Ctrl Pts',(-0.523552452478682,-1.70311144018918,
-2.08844961015169));
#14045=CARTESIAN_POINT('Ctrl Pts',(-0.384458109946442,-1.71569170964966,
-2.11823081535576));
#14046=CARTESIAN_POINT('Ctrl Pts',(-0.243879285742567,-1.72827204102101,
-2.1344480958084));
#14047=CARTESIAN_POINT('Ctrl Pts',(-0.230670163896899,-1.7294541189825,
-2.13597191018598));
#14048=CARTESIAN_POINT('Ctrl Pts',(-0.217447917878059,-1.73063619749059,
-2.13737593637491));
#14049=CARTESIAN_POINT('Ctrl Pts',(-0.204214801524846,-1.7318182765795,
-2.13865982929153));
#14050=CARTESIAN_POINT('Ctrl Pts',(-0.0940559936059023,-1.74165846991149,
-2.14934756976135));
#14051=CARTESIAN_POINT('Ctrl Pts',(0.0170319180460684,-1.75149860472723,
-2.15172318447799));
#14052=CARTESIAN_POINT('Ctrl Pts',(0.127629739073989,-1.76133870871583,
-2.14552092692591));
#14053=CARTESIAN_POINT('Ctrl Pts',(0.229677753696459,-1.77041811974203,
-2.13979813724087));
#14054=CARTESIAN_POINT('Ctrl Pts',(0.331307399421747,-1.77949750452303,
-2.12677281393757));
#14055=CARTESIAN_POINT('Ctrl Pts',(0.431398535636282,-1.78857688481002,
-2.10627522033382));
#14056=CARTESIAN_POINT('Ctrl Pts',(0.505667078849773,-1.79531386845012,
-2.09106581744455));
#14057=CARTESIAN_POINT('Ctrl Pts',(0.579088401370791,-1.80205084961592,
-2.07174320483138));
#14058=CARTESIAN_POINT('Ctrl Pts',(0.651268888525473,-1.80878783719349,
-2.04855194526834));
#14059=CARTESIAN_POINT('Ctrl Pts',(0.758244120422034,-1.81877240278462,
-2.01418129375952));
#14060=CARTESIAN_POINT('Ctrl Pts',(0.862440456081423,-1.82875703527447,
-1.97133727426226));
#14061=CARTESIAN_POINT('Ctrl Pts',(0.962751223328877,-1.83874168737687,
-1.92078030085791));
#14062=CARTESIAN_POINT('Ctrl Pts',(1.06496440405616,-1.84891570037515,-1.86926450448427));
#14063=CARTESIAN_POINT('Ctrl Pts',(1.16314447816446,-1.85908973373697,-1.80973982527943));
#14064=CARTESIAN_POINT('Ctrl Pts',(1.25610430924613,-1.86926373743437,-1.74296009602128));
#14065=CARTESIAN_POINT('Ctrl Pts',(1.3063395294205,-1.87476173920402,-1.70687252611682));
#14066=CARTESIAN_POINT('Ctrl Pts',(1.3550498964473,-1.8802597323108,-1.66866545866889));
#14067=CARTESIAN_POINT('Ctrl Pts',(1.40204415428096,-1.88575770885973,-1.62845284783459));
#14068=CARTESIAN_POINT('Ctrl Pts',(1.47814399737386,-1.89466082111193,-1.56333482031559));
#14069=CARTESIAN_POINT('Ctrl Pts',(1.54980220057176,-1.90356391843453,-1.49290076286398));
#14070=CARTESIAN_POINT('Ctrl Pts',(1.61607511600231,-1.91246700997469,-1.41772349525774));
#14071=CARTESIAN_POINT('Ctrl Pts',(1.65006518927242,-1.91703323030488,-1.3791665551023));
#14072=CARTESIAN_POINT('Ctrl Pts',(1.68263910959245,-1.92159944911403,-1.33936265105279));
#14073=CARTESIAN_POINT('Ctrl Pts',(1.7136730378829,-1.92616566763619,-1.29839312969576));
#14074=CARTESIAN_POINT('Ctrl Pts',(1.7741799371271,-1.93506843113624,-1.21851478888014));
#14075=CARTESIAN_POINT('Ctrl Pts',(1.82882984359509,-1.9439711935454,-1.13420417698836));
#14076=CARTESIAN_POINT('Ctrl Pts',(1.87730680081322,-1.95287396400987,-1.04651803924107));
#14077=CARTESIAN_POINT('Ctrl Pts',(1.89519082923519,-1.95615835744455,-1.01416903324573));
#14078=CARTESIAN_POINT('Ctrl Pts',(1.91223517668191,-1.95944275197557,-0.98136084759658));
#14079=CARTESIAN_POINT('Ctrl Pts',(1.92842564875693,-1.96272714806214,-0.948147166408794));
#14080=CARTESIAN_POINT('Ctrl Pts',(1.97707651191226,-1.97259645291104,-0.848343142729681));
#14081=CARTESIAN_POINT('Ctrl Pts',(2.01805448866746,-1.98246583113485,-0.744813178898148));
#14082=CARTESIAN_POINT('Ctrl Pts',(2.05102784716761,-1.99233522071939,-0.638793681783248));
#14083=CARTESIAN_POINT('Ctrl Pts',(2.08377938217068,-2.0021382154139,-0.533487415491025));
#14084=CARTESIAN_POINT('Ctrl Pts',(2.10863396352524,-2.01194122131676,-0.425723679332623));
#14085=CARTESIAN_POINT('Ctrl Pts',(2.12521884429204,-2.02174417765695,-0.31669842209029));
#14086=CARTESIAN_POINT('Ctrl Pts',(2.13534325322579,-2.0277284919335,-0.250142846325303));
#14087=CARTESIAN_POINT('Ctrl Pts',(2.14238491344303,-2.03371278773996,-0.183116928193918));
#14088=CARTESIAN_POINT('Ctrl Pts',(2.14624939550719,-2.03969705125123,-0.115893013806827));
#14089=CARTESIAN_POINT('Ctrl Pts',(2.15142844512317,-2.0477169610672,-0.0258017720281359));
#14090=CARTESIAN_POINT('Ctrl Pts',(2.1508970855676,-2.05573687209812,0.0646354082577172));
#14091=CARTESIAN_POINT('Ctrl Pts',(2.14443040646274,-2.06375678802137,0.154655204293321));
#14092=CARTESIAN_POINT('Ctrl Pts',(2.13690168346352,-2.07309384101008,0.259459246338326));
#14093=CARTESIAN_POINT('Ctrl Pts',(2.1213267628892,-2.08243090063007,0.363696511439923));
#14094=CARTESIAN_POINT('Ctrl Pts',(2.09820253713493,-2.09176797268451,0.466236306460128));
#14095=CARTESIAN_POINT('Ctrl Pts',(2.07764803655949,-2.10006744419787,0.557381164590559));
#14096=CARTESIAN_POINT('Ctrl Pts',(2.05112990792501,-2.10836692553559,0.647184319962309));
#14097=CARTESIAN_POINT('Ctrl Pts',(2.01902946446485,-2.11666642077307,0.73486384668651));
#14098=CARTESIAN_POINT('',(2.67614644529864,-2.1166752978846,0.974032799954154));
#14099=CARTESIAN_POINT('Ctrl Pts',(2.67638790329494,-2.11666698860102,0.974121792631881));
#14100=CARTESIAN_POINT('Ctrl Pts',(2.67638785912941,-2.08672748700797,0.974106749158961));
#14101=CARTESIAN_POINT('Ctrl Pts',(2.67157529235006,-2.05667767012892,0.972341928041461));
#14102=CARTESIAN_POINT('Ctrl Pts',(2.66268404270861,-2.02740880552684,0.969095274171888));
#14103=CARTESIAN_POINT('Ctrl Pts',(2.65402263405934,-1.99889654828049,0.965932547104144));
#14104=CARTESIAN_POINT('Ctrl Pts',(2.64149062979418,-1.97112535002398,0.961363588377978));
#14105=CARTESIAN_POINT('Ctrl Pts',(2.62579575237343,-1.9449566292807,0.95564659024295));
#14106=CARTESIAN_POINT('Ctrl Pts',(2.61159820845988,-1.92128447486024,0.950475009102186));
#14107=CARTESIAN_POINT('Ctrl Pts',(2.59481275799209,-1.89892397248532,0.944364084064225));
#14108=CARTESIAN_POINT('Ctrl Pts',(2.57598557478357,-1.87854093566211,0.937512918344076));
#14109=CARTESIAN_POINT('Ctrl Pts',(2.55503707155986,-1.85586127573259,0.92988980948147));
#14110=CARTESIAN_POINT('Ctrl Pts',(2.53155658992225,-1.83562899381035,0.921346468856337));
#14111=CARTESIAN_POINT('Ctrl Pts',(2.50636772427429,-1.81881930830857,0.912183426472423));
#14112=CARTESIAN_POINT('Ctrl Pts',(2.47882812394535,-1.80044086972207,0.9021652490532));
#14113=CARTESIAN_POINT('Ctrl Pts',(2.44924741230612,-1.78615580340538,0.891406679152019));
#14114=CARTESIAN_POINT('Ctrl Pts',(2.4187607069639,-1.77723122603903,0.880321667073218));
#14115=CARTESIAN_POINT('Ctrl Pts',(2.39592843838876,-1.77054738319471,0.872019819756467));
#14116=CARTESIAN_POINT('Ctrl Pts',(2.37258948914726,-1.76687025757582,0.863535408372535));
#14117=CARTESIAN_POINT('Ctrl Pts',(2.34923258819565,-1.76671767765912,0.855046590252549));
#14118=CARTESIAN_POINT('Ctrl Pts',(2.34872464986128,-1.76671435953105,0.854861985447934));
#14119=CARTESIAN_POINT('Ctrl Pts',(2.34821668840943,-1.76671270731511,0.854677371654798));
#14120=CARTESIAN_POINT('Ctrl Pts',(2.34770870905014,-1.76671272653744,0.854492750764122));
#14121=CARTESIAN_POINT('Ctrl Pts',(2.32259204314204,-1.76671367697138,0.845364306574461));
#14122=CARTESIAN_POINT('Ctrl Pts',(2.29743124275574,-1.77080593190913,0.836218370574714));
#14123=CARTESIAN_POINT('Ctrl Pts',(2.27285936173094,-1.77837665826544,0.827284778016346));
#14124=CARTESIAN_POINT('Ctrl Pts',(2.24680917535251,-1.78640285831105,0.817813718355116));
#14125=CARTESIAN_POINT('Ctrl Pts',(2.22142265714173,-1.79833745252292,0.808581961916408));
#14126=CARTESIAN_POINT('Ctrl Pts',(2.19744399945536,-1.81339165766342,0.79985981724167));
#14127=CARTESIAN_POINT('Ctrl Pts',(2.17404994367491,-1.82807883988161,0.791350319265811));
#14128=CARTESIAN_POINT('Ctrl Pts',(2.15199742940655,-1.8457334718391,0.783326435636173));
#14129=CARTESIAN_POINT('Ctrl Pts',(2.13194384484284,-1.86559379902691,0.776026983036747));
#14130=CARTESIAN_POINT('Ctrl Pts',(2.12820384737706,-1.86929775395406,0.774665633691115));
#14131=CARTESIAN_POINT('Ctrl Pts',(2.12453324555184,-1.87307838964054,0.773329433815644));
#14132=CARTESIAN_POINT('Ctrl Pts',(2.12093610725898,-1.87693072872798,0.772019861055125));
#14133=CARTESIAN_POINT('Ctrl Pts',(2.09876788439411,-1.90067168737027,0.763949306506105));
#14134=CARTESIAN_POINT('Ctrl Pts',(2.07936467035814,-1.92715926223815,0.756883690562579));
#14135=CARTESIAN_POINT('Ctrl Pts',(2.06360873957658,-1.95534911991786,0.75114346667111));
#14136=CARTESIAN_POINT('Ctrl Pts',(2.04587070830782,-1.98708526955682,0.744681121012945));
#14137=CARTESIAN_POINT('Ctrl Pts',(2.03275442850618,-2.02097909692896,0.739898298179565));
#14138=CARTESIAN_POINT('Ctrl Pts',(2.02549893555319,-2.05560715796329,0.737244850782333));
#14139=CARTESIAN_POINT('Ctrl Pts',(2.02126782786752,-2.07580083138167,0.735697468440612));
#14140=CARTESIAN_POINT('Ctrl Pts',(2.01902953634433,-2.09624540533448,0.734874123352453));
#14141=CARTESIAN_POINT('Ctrl Pts',(2.01902946446485,-2.11666642077307,0.73486384668651));
#14142=CARTESIAN_POINT('Ctrl Pts',(-2.80458233589288,2.11665724005696,-0.494527021640491));
#14143=CARTESIAN_POINT('Ctrl Pts',(-2.78195692265552,2.10782585092188,-0.624275021078974));
#14144=CARTESIAN_POINT('Ctrl Pts',(-2.75048104123089,2.09899509849822,-0.752587818575418));
#14145=CARTESIAN_POINT('Ctrl Pts',(-2.71025331183979,2.09016408935099,-0.878085114837578));
#14146=CARTESIAN_POINT('Ctrl Pts',(-2.67015244924239,2.08136093068979,-1.00318662839371));
#14147=CARTESIAN_POINT('Ctrl Pts',(-2.62135498898967,2.07255751692177,-1.12548915070111));
#14148=CARTESIAN_POINT('Ctrl Pts',(-2.56400948500098,2.06375296303797,-1.243633861005));
#14149=CARTESIAN_POINT('Ctrl Pts',(-2.52310745426962,2.05747306124127,-1.32790129673196));
#14150=CARTESIAN_POINT('Ctrl Pts',(-2.47785791614011,2.05119257942859,-1.41005369783363));
#14151=CARTESIAN_POINT('Ctrl Pts',(-2.42862419207533,2.04491119646754,-1.48974196812404));
#14152=CARTESIAN_POINT('Ctrl Pts',(-2.35656441161157,2.03571759826265,-1.60637582777495));
#14153=CARTESIAN_POINT('Ctrl Pts',(-2.27600690970338,2.02652406927197,-1.71768368532288));
#14154=CARTESIAN_POINT('Ctrl Pts',(-2.18800206838966,2.01733111013869,-1.82275301439088));
#14155=CARTESIAN_POINT('Ctrl Pts',(-2.09783558126732,2.00791234613738,-1.93040314096281));
#14156=CARTESIAN_POINT('Ctrl Pts',(-1.99985064780579,1.99849418033187,-2.03150549829407));
#14157=CARTESIAN_POINT('Ctrl Pts',(-1.89512935512655,1.98907715117062,-2.1250528185535));
#14158=CARTESIAN_POINT('Ctrl Pts',(-1.83610060721461,1.98376900966265,-2.1777830804148));
#14159=CARTESIAN_POINT('Ctrl Pts',(-1.77493073132476,1.97846122929977,-2.22811233864566));
#14160=CARTESIAN_POINT('Ctrl Pts',(-1.71180854829565,1.97315390651591,-2.27585485864977));
#14161=CARTESIAN_POINT('Ctrl Pts',(-1.61043745719953,1.96463060970357,-2.35252697473078));
#14162=CARTESIAN_POINT('Ctrl Pts',(-1.50392997092724,1.95610753076537,-2.42259747247663));
#14163=CARTESIAN_POINT('Ctrl Pts',(-1.39318682599955,1.94758406792774,-2.48516487943052));
#14164=CARTESIAN_POINT('Ctrl Pts',(-1.30044328685753,1.9404459637153,-2.53756291056491));
#14165=CARTESIAN_POINT('Ctrl Pts',(-1.20473011838826,1.93330759025575,-2.58469891486034));
#14166=CARTESIAN_POINT('Ctrl Pts',(-1.10659388581258,1.92616859409453,-2.62606546345969));
#14167=CARTESIAN_POINT('Ctrl Pts',(-0.993148428790342,1.91791591655705,
-2.67388518190738));
#14168=CARTESIAN_POINT('Ctrl Pts',(-0.876465346112244,1.90966240688131,
-2.71399381805545));
#14169=CARTESIAN_POINT('Ctrl Pts',(-0.757696549627284,1.90140751904957,
-2.7463426951939));
#14170=CARTESIAN_POINT('Ctrl Pts',(-0.626181159144015,1.89226669394469,
-2.78216334282587));
#14171=CARTESIAN_POINT('Ctrl Pts',(-0.492130004822071,1.88312627592044,
-2.80847279982899));
#14172=CARTESIAN_POINT('Ctrl Pts',(-0.356898911517837,1.87398652541256,
-2.82527490060671));
#14173=CARTESIAN_POINT('Ctrl Pts',(-0.21960563696361,1.86470739998973,-2.84233322187587));
#14174=CARTESIAN_POINT('Ctrl Pts',(-0.0810949057590346,1.85542896259683,
-2.8495921840046));
#14175=CARTESIAN_POINT('Ctrl Pts',(0.0572283211157545,1.84615148576666,
-2.84700464260265));
#14176=CARTESIAN_POINT('Ctrl Pts',(0.139230104201676,1.84065154436274,-2.84547067745765));
#14177=CARTESIAN_POINT('Ctrl Pts',(0.221166160679518,1.83515194054302,-2.8404752344192));
#14178=CARTESIAN_POINT('Ctrl Pts',(0.30274321958312,1.8296527310885,-2.83199983632318));
#14179=CARTESIAN_POINT('Ctrl Pts',(0.42569985615815,1.82136407362233,-2.81922533258981));
#14180=CARTESIAN_POINT('Ctrl Pts',(0.547929990333508,1.81307516416304,-2.79853030292443));
#14181=CARTESIAN_POINT('Ctrl Pts',(0.668253724755781,1.8047857434996,-2.76984910916053));
#14182=CARTESIAN_POINT('Ctrl Pts',(0.746648213223421,1.79938493961228,-2.75116245914457));
#14183=CARTESIAN_POINT('Ctrl Pts',(0.82423327113268,1.79398391872342,-2.72908680139804));
#14184=CARTESIAN_POINT('Ctrl Pts',(0.900683703946973,1.78858260914337,-2.70361587160169));
#14185=CARTESIAN_POINT('Ctrl Pts',(1.01786233849029,1.78030380602824,-2.66457555928147));
#14186=CARTESIAN_POINT('Ctrl Pts',(1.13237393427125,1.77202432469325,-2.61755666473922));
#14187=CARTESIAN_POINT('Ctrl Pts',(1.24330248133285,1.76374390699457,-2.56329332031478));
#14188=CARTESIAN_POINT('Ctrl Pts',(1.26938375238872,1.76179703376693,-2.55053504454339));
#14189=CARTESIAN_POINT('Ctrl Pts',(1.2952670635135,1.75985010877677,-2.53737649080999));
#14190=CARTESIAN_POINT('Ctrl Pts',(1.3209407377059,1.75790312866889,-2.52382754784158));
#14191=CARTESIAN_POINT('Ctrl Pts',(1.44045818507747,1.74883944378948,-2.46075379119761));
#14192=CARTESIAN_POINT('Ctrl Pts',(1.55546286758081,1.73977653023493,-2.38920902392338));
#14193=CARTESIAN_POINT('Ctrl Pts',(1.66496510134029,1.73071439590768,-2.31005428671678));
#14194=CARTESIAN_POINT('Ctrl Pts',(1.77514668187161,1.72159604052,-2.23040847719732));
#14195=CARTESIAN_POINT('Ctrl Pts',(1.87975834022544,1.7124784740582,-2.14305722122181));
#14196=CARTESIAN_POINT('Ctrl Pts',(1.97776537519384,1.70336170457275,-2.04883305684583));
#14197=CARTESIAN_POINT('Ctrl Pts',(2.0394413901976,1.69762450405697,-1.98953760955835));
#14198=CARTESIAN_POINT('Ctrl Pts',(2.09850125673617,1.69188761916048,-1.92751949672681));
#14199=CARTESIAN_POINT('Ctrl Pts',(2.15467902364597,1.68615105188955,-1.86297929705858));
#14200=CARTESIAN_POINT('Ctrl Pts',(2.23506632755639,1.67794233869256,-1.77062581042926));
#14201=CARTESIAN_POINT('Ctrl Pts',(2.30958423117854,1.66973293664819,-1.67306262287684));
#14202=CARTESIAN_POINT('Ctrl Pts',(2.37733115154558,1.66152289082693,-1.57100557093827));
#14203=CARTESIAN_POINT('Ctrl Pts',(2.40628489938846,1.65801407307995,-1.5273883241113));
#14204=CARTESIAN_POINT('Ctrl Pts',(2.43400232755433,1.6545051377442,-1.48295073002168));
#14205=CARTESIAN_POINT('Ctrl Pts',(2.46041525696606,1.65099608833801,-1.43775059105066));
#14206=CARTESIAN_POINT('Ctrl Pts',(2.52223089679436,1.64278366589703,-1.3319662054088));
#14207=CARTESIAN_POINT('Ctrl Pts',(2.57689806784256,1.63457061866224,-1.22200385757481));
#14208=CARTESIAN_POINT('Ctrl Pts',(2.6242135385369,1.62635699173425,-1.1089945602547));
#14209=CARTESIAN_POINT('Ctrl Pts',(2.64717459106986,1.62237111741847,-1.05415388395152));
#14210=CARTESIAN_POINT('Ctrl Pts',(2.66840510749953,1.61838510658923,-0.998595985561653));
#14211=CARTESIAN_POINT('Ctrl Pts',(2.68788611968169,1.61439896440059,-0.942451252524915));
#14212=CARTESIAN_POINT('Ctrl Pts',(2.73243195458445,1.6052841386321,-0.814069113797786));
#14213=CARTESIAN_POINT('Ctrl Pts',(2.76786121198766,1.59617037125586,-0.682546337603376));
#14214=CARTESIAN_POINT('Ctrl Pts',(2.79398463412037,1.58705744696499,-0.549200789547298));
#14215=CARTESIAN_POINT('Ctrl Pts',(2.82004885042824,1.57796517610141,-0.41615745431471));
#14216=CARTESIAN_POINT('Ctrl Pts',(2.83684955611659,1.56887374450604,-0.281298348456388));
#14217=CARTESIAN_POINT('Ctrl Pts',(2.84414931768941,1.5597829383326,-0.145920560005815));
#14218=CARTESIAN_POINT('Ctrl Pts',(2.84873544117182,1.55407157923543,-0.060868569140493));
#14219=CARTESIAN_POINT('Ctrl Pts',(2.84957048782428,1.54836046699627,0.0243883193675018));
#14220=CARTESIAN_POINT('Ctrl Pts',(2.84658502904739,1.54264954858617,0.109527498678143));
#14221=CARTESIAN_POINT('Ctrl Pts',(2.84224367557131,1.5343449236209,0.23333402212198));
#14222=CARTESIAN_POINT('Ctrl Pts',(2.82981710043464,1.52603917879535,0.356908951255374));
#14223=CARTESIAN_POINT('Ctrl Pts',(2.80910367996215,1.5177326713053,0.479083523772095));
#14224=CARTESIAN_POINT('Ctrl Pts',(2.80551079386501,1.51629185010841,0.500275548701168));
#14225=CARTESIAN_POINT('Ctrl Pts',(2.80166870570173,1.51485100596501,0.521425439142127));
#14226=CARTESIAN_POINT('Ctrl Pts',(2.79757652440072,1.51341014073923,0.54252710241733));
#14227=CARTESIAN_POINT('Ctrl Pts',(2.77394067383935,1.50508791045412,0.664407274159863));
#14228=CARTESIAN_POINT('Ctrl Pts',(2.74195745366128,1.49676497685038,0.784677265492543));
#14229=CARTESIAN_POINT('Ctrl Pts',(2.70223914758,1.48844169912296,0.902317170192954));
#14230=CARTESIAN_POINT('Ctrl Pts',(2.67432890489442,1.48259289225702,0.98498329102345));
#14231=CARTESIAN_POINT('Ctrl Pts',(2.64260028236357,1.47674391546488,1.06635087545059));
#14232=CARTESIAN_POINT('Ctrl Pts',(2.60727944653752,1.4708948933841,1.14607297111354));
#14233=CARTESIAN_POINT('Ctrl Pts',(2.55107174904667,1.46158707107342,1.2729384693828));
#14234=CARTESIAN_POINT('Ctrl Pts',(2.48572431206794,1.45228057614097,1.39575090488485));
#14235=CARTESIAN_POINT('Ctrl Pts',(2.41200087454017,1.44297495438738,1.51331153309315));
#14236=CARTESIAN_POINT('Ctrl Pts',(2.33912082498289,1.43377578791732,1.62952728071858));
#14237=CARTESIAN_POINT('Ctrl Pts',(2.2580545758542,1.42457747476227,1.74061172045069));
#14238=CARTESIAN_POINT('Ctrl Pts',(2.16949824700251,1.41537957613314,1.84537958337022));
#14239=CARTESIAN_POINT('Ctrl Pts',(2.11740532649016,1.40996894757185,1.90700887656795));
#14240=CARTESIAN_POINT('Ctrl Pts',(2.06271985469377,1.40455846245042,1.96645183280968));
#14241=CARTESIAN_POINT('Ctrl Pts',(2.00557821089282,1.39914803145207,2.02346054546564));
#14242=CARTESIAN_POINT('Ctrl Pts',(1.92348429671894,1.39137500588827,2.10536348091922));
#14243=CARTESIAN_POINT('Ctrl Pts',(1.83633357380992,1.38360069944669,2.18222360846758));
#14244=CARTESIAN_POINT('Ctrl Pts',(1.74463343531627,1.37582563843094,2.25322530463692));
#14245=CARTESIAN_POINT('Ctrl Pts',(1.64304360701143,1.36721205150921,2.33188440201326));
#14246=CARTESIAN_POINT('Ctrl Pts',(1.53587039232361,1.3585975384778,2.40335199327399));
#14247=CARTESIAN_POINT('Ctrl Pts',(1.42435621965327,1.34998281494774,2.46723143747144));
#14248=CARTESIAN_POINT('Ctrl Pts',(1.32687558837224,1.34245221441587,2.52307194991157));
#14249=CARTESIAN_POINT('Ctrl Pts',(1.22607884688904,1.33492145303225,2.57311451942267));
#14250=CARTESIAN_POINT('Ctrl Pts',(1.12280743727165,1.32739100881219,2.61712470493613));
#14251=CARTESIAN_POINT('Ctrl Pts',(0.990207240359367,1.31772193980155,2.67363365825489));
#14252=CARTESIAN_POINT('Ctrl Pts',(0.853379606627105,1.30805447587311,2.72026934000668));
#14253=CARTESIAN_POINT('Ctrl Pts',(0.713861018160752,1.29838786904702,2.75656592271339));
#14254=CARTESIAN_POINT('Ctrl Pts',(0.577367304017838,1.28893084197014,2.79207556654503));
#14255=CARTESIAN_POINT('Ctrl Pts',(0.438296805635782,1.27947463523317,2.81768977284684));
#14256=CARTESIAN_POINT('Ctrl Pts',(0.298080367904077,1.27001854845938,2.83292424809103));
#14257=CARTESIAN_POINT('Ctrl Pts',(0.227042875518054,1.26522783559389,2.84064245101125));
#14258=CARTESIAN_POINT('Ctrl Pts',(0.155711241883743,1.2604371535195,2.84569568310527));
#14259=CARTESIAN_POINT('Ctrl Pts',(0.0842722593669868,1.25564641116154,
2.84801583840595));
#14260=CARTESIAN_POINT('Ctrl Pts',(-0.00222290094123247,1.24984599220751,
2.85082497982428));
#14261=CARTESIAN_POINT('Ctrl Pts',(-0.0888424845338625,1.24404474795043,
2.84962541460311));
#14262=CARTESIAN_POINT('Ctrl Pts',(-0.17521088761524,1.23824297558038,2.84430505124541));
#14263=CARTESIAN_POINT('Ctrl Pts',(-0.311666308540717,1.22907662234674,
2.8358992871517));
#14264=CARTESIAN_POINT('Ctrl Pts',(-0.447493850899554,1.21990895086045,
2.81720476888644));
#14265=CARTESIAN_POINT('Ctrl Pts',(-0.581278969526878,1.21074113316035,
2.78884600173747));
#14266=CARTESIAN_POINT('Ctrl Pts',(-0.711907039215729,1.20178965678008,
2.76115644217036));
#14267=CARTESIAN_POINT('Ctrl Pts',(-0.840586922470479,1.19283804100528,
2.72425404482427));
#14268=CARTESIAN_POINT('Ctrl Pts',(-0.966020705809652,1.18388737684435,
2.67876424010694));
#14269=CARTESIAN_POINT('Ctrl Pts',(-1.11059363914152,1.17357098728354,2.62633343295434));
#14270=CARTESIAN_POINT('Ctrl Pts',(-1.25105662977625,1.16325655063408,2.56243126293453));
#14271=CARTESIAN_POINT('Ctrl Pts',(-1.3856020394883,1.15294287837623,2.48785423186171));
#14272=CARTESIAN_POINT('Ctrl Pts',(-1.5155161453378,1.14298422194736,2.41584428124748));
#14273=CARTESIAN_POINT('Ctrl Pts',(-1.63991404568272,1.13302627819219,2.33388097949739));
#14274=CARTESIAN_POINT('Ctrl Pts',(-1.75713727350267,1.12306797714789,2.24264513907806));
#14275=CARTESIAN_POINT('Ctrl Pts',(-1.799997721801,1.11942691338445,2.20928648572948));
#14276=CARTESIAN_POINT('Ctrl Pts',(-1.84189863558586,1.11578580185645,2.17468791758819));
#14277=CARTESIAN_POINT('Ctrl Pts',(-1.8827574653352,1.11214459026435,2.13888172789186));
#14278=CARTESIAN_POINT('Ctrl Pts',(-1.92570430221763,1.10831730198274,2.10124573592381));
#14279=CARTESIAN_POINT('Ctrl Pts',(-1.96748293849158,1.10448963806102,2.06229011400923));
#14280=CARTESIAN_POINT('Ctrl Pts',(-2.00799362759083,1.10066169833689,2.02206122998739));
#14281=CARTESIAN_POINT('Ctrl Pts',(-2.1158473025442,1.09047037905974,1.91495781907288));
#14282=CARTESIAN_POINT('Ctrl Pts',(-2.21471041744568,1.08027710486391,1.79882743654177));
#14283=CARTESIAN_POINT('Ctrl Pts',(-2.30372169493775,1.07008375979099,1.67556698066195));
#14284=CARTESIAN_POINT('Ctrl Pts',(-2.39017505429039,1.06018334099661,1.55584866196802));
#14285=CARTESIAN_POINT('Ctrl Pts',(-2.4673343500471,1.05028285534021,1.42940544772771));
#14286=CARTESIAN_POINT('Ctrl Pts',(-2.53445489838778,1.04038402906109,1.29799088753696));
#14287=CARTESIAN_POINT('Ctrl Pts',(-2.61554686873761,1.02842472081692,1.13922183868422));
#14288=CARTESIAN_POINT('Ctrl Pts',(-2.68213302783367,1.01646812482486,0.972930314429998));
#14289=CARTESIAN_POINT('Ctrl Pts',(-2.7328636458305,1.0045119563375,0.801945004864593));
#14290=CARTESIAN_POINT('Ctrl Pts',(-2.77931928941865,0.993563311833254,
0.64536830791847));
#14291=CARTESIAN_POINT('Ctrl Pts',(-2.81247886793264,0.982615025819403,
0.484854447140363));
#14292=CARTESIAN_POINT('Ctrl Pts',(-2.83125821150622,0.97166534383724,0.322581819316084));
#14293=CARTESIAN_POINT('Ctrl Pts',(-2.83298633767105,0.970657724382605,
0.307649051678014));
#14294=CARTESIAN_POINT('Ctrl Pts',(-2.83459265425157,0.96965009310666,0.292701401630804));
#14295=CARTESIAN_POINT('Ctrl Pts',(-2.83607629458685,0.968642448642216,
0.277740574396832));
#14296=CARTESIAN_POINT('Ctrl Pts',(-2.83880587230564,0.966788600500464,
0.250215884146019));
#14297=CARTESIAN_POINT('Ctrl Pts',(-2.84111956607568,0.96493467000898,0.222653121347949));
#14298=CARTESIAN_POINT('Ctrl Pts',(-2.84301252487888,0.96308066892502,0.195063450417379));
#14299=CARTESIAN_POINT('Ctrl Pts',(-2.85561123541669,0.950741244023576,
0.0114385995752131));
#14300=CARTESIAN_POINT('Ctrl Pts',(-2.84956951455601,0.938398692119184,
-0.173376147093211));
#14301=CARTESIAN_POINT('Ctrl Pts',(-2.82597651771739,0.926056479468952,
-0.355930500791568));
#14302=CARTESIAN_POINT('Ctrl Pts',(-2.80738470726687,0.916330539195121,
-0.499787424271555));
#14303=CARTESIAN_POINT('Ctrl Pts',(-2.7778948576424,0.906604809591102,-0.642240748807444));
#14304=CARTESIAN_POINT('Ctrl Pts',(-2.73805633784352,0.896880986854682,
-0.781618227284983));
#14305=CARTESIAN_POINT('Ctrl Pts',(-2.68219190584366,0.883245544655029,
-0.977063331872888));
#14306=CARTESIAN_POINT('Ctrl Pts',(-2.60587050090985,0.869613649916618,
-1.16685079029084));
#14307=CARTESIAN_POINT('Ctrl Pts',(-2.510357866132,0.855981266040079,-1.3463984534859));
#14308=CARTESIAN_POINT('Ctrl Pts',(-2.43917350435211,0.845821222313435,
-1.48021306181849));
#14309=CARTESIAN_POINT('Ctrl Pts',(-2.35732930885754,0.835660906893434,
-1.60833903565359));
#14310=CARTESIAN_POINT('Ctrl Pts',(-2.26535011224914,0.825498648739708,
-1.72886054990566));
#14311=CARTESIAN_POINT('Ctrl Pts',(-2.26426761998683,0.82537905032806,-1.73027895332111));
#14312=CARTESIAN_POINT('Ctrl Pts',(-2.26318372397246,0.825259451647331,
-1.73169630326915));
#14313=CARTESIAN_POINT('Ctrl Pts',(-2.26209842687303,0.825139852694796,
-1.73311259799423));
#14314=CARTESIAN_POINT('Ctrl Pts',(-2.14142969266093,0.811842245778572,
-1.89058329596036));
#14315=CARTESIAN_POINT('Ctrl Pts',(-2.00366546403506,0.798541291076087,
-2.03472132532182));
#14316=CARTESIAN_POINT('Ctrl Pts',(-1.85262348342731,0.785240915843383,
-2.16327288912423));
#14317=CARTESIAN_POINT('Ctrl Pts',(-1.73199858567728,0.774618992084,-2.26593652725237));
#14318=CARTESIAN_POINT('Ctrl Pts',(-1.60290395110196,0.763997437905361,
-2.3586595711926));
#14319=CARTESIAN_POINT('Ctrl Pts',(-1.46726066438,0.75337825366249,-2.44029700691361));
#14320=CARTESIAN_POINT('Ctrl Pts',(-1.31445136477984,0.741415183866013,
-2.53226587374926));
#14321=CARTESIAN_POINT('Ctrl Pts',(-1.15306195631937,0.729454649678202,
-2.61032190563498));
#14322=CARTESIAN_POINT('Ctrl Pts',(-0.985839578997115,0.717493702838762,
-2.67265181028179));
#14323=CARTESIAN_POINT('Ctrl Pts',(-0.848015707358323,0.707635548515908,
-2.72402381512266));
#14324=CARTESIAN_POINT('Ctrl Pts',(-0.706230953840882,0.697777113879811,
-2.76471322800078));
#14325=CARTESIAN_POINT('Ctrl Pts',(-0.562044485381816,0.687916748276768,
-2.79372079692265));
#14326=CARTESIAN_POINT('Ctrl Pts',(-0.531435194482997,0.685823494989287,
-2.79987880276665));
#14327=CARTESIAN_POINT('Ctrl Pts',(-0.500717716471415,0.683730154679143,
-2.80551040642833));
#14328=CARTESIAN_POINT('Ctrl Pts',(-0.469909449984022,0.681636711554149,
-2.81061812312463));
#14329=CARTESIAN_POINT('Ctrl Pts',(-0.311384277657102,0.670864815891595,
-2.83690008448744));
#14330=CARTESIAN_POINT('Ctrl Pts',(-0.150671980668343,0.660091482015627,
-2.84927975948678));
#14331=CARTESIAN_POINT('Ctrl Pts',(0.0099591028400281,0.64931841187939,
-2.84821053083917));
#14332=CARTESIAN_POINT('Ctrl Pts',(0.17896284199308,0.637983811530465,-2.84708557024308));
#14333=CARTESIAN_POINT('Ctrl Pts',(0.34787789599397,0.626649503131862,-2.83107334950554));
#14334=CARTESIAN_POINT('Ctrl Pts',(0.51408428978591,0.615317468884971,-2.80064983867025));
#14335=CARTESIAN_POINT('Ctrl Pts',(0.540689324805138,0.613503524420505,
-2.79577987817887));
#14336=CARTESIAN_POINT('Ctrl Pts',(0.567224975267696,0.61168963822693,-2.79054054879862));
#14337=CARTESIAN_POINT('Ctrl Pts',(0.59368050928722,0.609875818434349,-2.78493368240782));
#14338=CARTESIAN_POINT('Ctrl Pts',(0.739823533721816,0.599856095904029,
-2.75396078988004));
#14339=CARTESIAN_POINT('Ctrl Pts',(0.883727347479231,0.589837817515454,
-2.71172418574845));
#14340=CARTESIAN_POINT('Ctrl Pts',(1.02342699697088,0.579819329519902,-2.65849030561885));
#14341=CARTESIAN_POINT('Ctrl Pts',(1.16046079679312,0.569992021552417,-2.60627227286081));
#14342=CARTESIAN_POINT('Ctrl Pts',(1.29344805073623,0.560164511901412,-2.54347303709899));
#14343=CARTESIAN_POINT('Ctrl Pts',(1.42053874146158,0.550335239697112,-2.47039258642219));
#14344=CARTESIAN_POINT('Ctrl Pts',(1.47312477640536,0.546268203404703,-2.44015424944357));
#14345=CARTESIAN_POINT('Ctrl Pts',(1.52470146343064,0.54220086535649,-2.40815628242956));
#14346=CARTESIAN_POINT('Ctrl Pts',(1.57518338415778,0.538133114982619,-2.37449979056686));
#14347=CARTESIAN_POINT('Ctrl Pts',(1.69729820182146,0.528293303262863,-2.29308536916979));
#14348=CARTESIAN_POINT('Ctrl Pts',(1.81289131980392,0.518452892961791,-2.20204937750933));
#14349=CARTESIAN_POINT('Ctrl Pts',(1.92091735073199,0.508612868932424,-2.10277545645514));
#14350=CARTESIAN_POINT('Ctrl Pts',(2.03287349302946,0.498414853500606,-1.99988983586455));
#14351=CARTESIAN_POINT('Ctrl Pts',(2.13670294434962,0.488217252957753,-1.88815519413113));
#14352=CARTESIAN_POINT('Ctrl Pts',(2.23121668812399,0.478021163605228,-1.76906264376533));
#14353=CARTESIAN_POINT('Ctrl Pts',(2.26720817603854,0.474138422195861,-1.72371137615037));
#14354=CARTESIAN_POINT('Ctrl Pts',(2.30184842051047,0.470255899930118,-1.67729267913346));
#14355=CARTESIAN_POINT('Ctrl Pts',(2.33507036011353,0.466373657348281,-1.62988750356013));
#14356=CARTESIAN_POINT('Ctrl Pts',(2.41273176910905,0.457298316396783,-1.51907059242573));
#14357=CARTESIAN_POINT('Ctrl Pts',(2.48273157246174,0.448223760354261,-1.40272772949553));
#14358=CARTESIAN_POINT('Ctrl Pts',(2.54408129257416,0.4391489482232,-1.28199626892511));
#14359=CARTESIAN_POINT('Ctrl Pts',(2.60356074674044,0.430350784658185,-1.16494534575437));
#14360=CARTESIAN_POINT('Ctrl Pts',(2.65490892647938,0.421552380380548,-1.04377036445469));
#14361=CARTESIAN_POINT('Ctrl Pts',(2.69726206377657,0.412752786725291,-0.919536395873714));
#14362=CARTESIAN_POINT('Ctrl Pts',(2.72633564009712,0.406712250556015,-0.83425521016603));
#14363=CARTESIAN_POINT('Ctrl Pts',(2.75117138033395,0.400671153925594,-0.747533168042571));
#14364=CARTESIAN_POINT('Ctrl Pts',(2.7717797395978,0.394629189966113,-0.659813786973422));
#14365=CARTESIAN_POINT('Ctrl Pts',(2.80375197296895,0.385255562533699,-0.523724130984334));
#14366=CARTESIAN_POINT('Ctrl Pts',(2.82553726556799,0.375881893634451,-0.385313547487032));
#14367=CARTESIAN_POINT('Ctrl Pts',(2.83724652168304,0.366508758774783,-0.246056202140706));
#14368=CARTESIAN_POINT('Ctrl Pts',(2.84925229116111,0.356898268124789,-0.103272444579225));
#14369=CARTESIAN_POINT('Ctrl Pts',(2.85066541482192,0.347288338903776,0.0404027634423335));
#14370=CARTESIAN_POINT('Ctrl Pts',(2.84155340634652,0.337679591455343,0.18339543013698));
#14371=CARTESIAN_POINT('Ctrl Pts',(2.83687230357611,0.332743299481687,0.256854906170083));
#14372=CARTESIAN_POINT('Ctrl Pts',(2.82941258685957,0.32780731939845,0.330134368779524));
#14373=CARTESIAN_POINT('Ctrl Pts',(2.81917806754171,0.322871735313071,0.403020188466609));
#14374=CARTESIAN_POINT('Ctrl Pts',(2.80142248463043,0.314309127757034,0.529467769864187));
#14375=CARTESIAN_POINT('Ctrl Pts',(2.77529267449128,0.305746785348526,0.654854651051419));
#14376=CARTESIAN_POINT('Ctrl Pts',(2.74079858797234,0.297184076994133,0.777892924300791));
#14377=CARTESIAN_POINT('Ctrl Pts',(2.71123783404779,0.289846004294255,0.883334305298909));
#14378=CARTESIAN_POINT('Ctrl Pts',(2.675535086332,0.282507662838135,0.987050215039095));
#14379=CARTESIAN_POINT('Ctrl Pts',(2.63372688779794,0.275168655428478,1.08823367223257));
#14380=CARTESIAN_POINT('Ctrl Pts',(2.58807592749233,0.267155089963133,1.19871731299886));
#14381=CARTESIAN_POINT('Ctrl Pts',(2.53514542312535,0.259140730497123,1.30618070531776));
#14382=CARTESIAN_POINT('Ctrl Pts',(2.47565204537744,0.251125059933902,1.40985110762689));
#14383=CARTESIAN_POINT('Ctrl Pts',(2.40780838796007,0.241984338256172,1.52807232021941));
#14384=CARTESIAN_POINT('Ctrl Pts',(2.33145002966693,0.232843999637142,1.64134427148275));
#14385=CARTESIAN_POINT('Ctrl Pts',(2.24754333145362,0.223704325212609,1.74871557175885));
#14386=CARTESIAN_POINT('Ctrl Pts',(2.16228962806164,0.214417926044483,1.85781056871938));
#14387=CARTESIAN_POINT('Ctrl Pts',(2.06924251621642,0.205132212567469,1.96081494828424));
#14388=CARTESIAN_POINT('Ctrl Pts',(1.96936951706988,0.195847479675699,2.0567044677364));
#14389=CARTESIAN_POINT('Ctrl Pts',(1.91028458189457,0.190354625293452,2.11343277357719));
#14390=CARTESIAN_POINT('Ctrl Pts',(1.84880982925535,0.184862114107581,2.16767036869738));
#14391=CARTESIAN_POINT('Ctrl Pts',(1.78513987983399,0.179370007177408,2.21919873359685));
#14392=CARTESIAN_POINT('Ctrl Pts',(1.68894916907077,0.171072691504912,2.29704629102687));
#14393=CARTESIAN_POINT('Ctrl Pts',(1.58767192555512,0.162775177956397,2.3687647574989));
#14394=CARTESIAN_POINT('Ctrl Pts',(1.48210122139711,0.154477168518722,2.43347386498712));
#14395=CARTESIAN_POINT('Ctrl Pts',(1.41045945317825,0.148846022325721,2.47738637762303));
#14396=CARTESIAN_POINT('Ctrl Pts',(1.33684137980812,0.143214647767288,2.51807155841732));
#14397=CARTESIAN_POINT('Ctrl Pts',(1.26150357893371,0.137582951710285,2.55526488394704));
#14398=CARTESIAN_POINT('Ctrl Pts',(1.15066666393052,0.129297604780205,2.60998367600861));
#14399=CARTESIAN_POINT('Ctrl Pts',(1.03610718865871,0.121011561989863,2.6571422134355));
#14400=CARTESIAN_POINT('Ctrl Pts',(0.918995430112488,0.112724526775131,
2.696618264617));
#14401=CARTESIAN_POINT('Ctrl Pts',(0.894954400175827,0.111023340966322,
2.7047220190138));
#14402=CARTESIAN_POINT('Ctrl Pts',(0.870805859448953,0.109322113335728,
2.71250219525392));
#14403=CARTESIAN_POINT('Ctrl Pts',(0.846559984942935,0.107620841317824,
2.71995800043706));
#14404=CARTESIAN_POINT('Ctrl Pts',(0.717441227963609,0.0985609029691008,
2.75966307674962));
#14405=CARTESIAN_POINT('Ctrl Pts',(0.585538508374012,0.0895016936606722,
2.79018113528876));
#14406=CARTESIAN_POINT('Ctrl Pts',(0.452160387528534,0.0804432509080095,
2.81142975491808));
#14407=CARTESIAN_POINT('Ctrl Pts',(0.317796625702479,0.0713178678480413,
2.83283539812933));
#14408=CARTESIAN_POINT('Ctrl Pts',(0.181934324020822,0.0621932627151443,
2.84483427845823));
#14409=CARTESIAN_POINT('Ctrl Pts',(0.0458981191767985,0.0530694738626992,
2.84729178064325));
#14410=CARTESIAN_POINT('Ctrl Pts',(-0.0395963040053689,0.0473354630817454,
2.8488362425166));
#14411=CARTESIAN_POINT('Ctrl Pts',(-0.125159610904366,0.0416017747088944,
2.84661111327967));
#14412=CARTESIAN_POINT('Ctrl Pts',(-0.210462215375585,0.0358684182644795,
2.84057242424866));
#14413=CARTESIAN_POINT('Ctrl Pts',(-0.332628311613721,0.0276573937653124,
2.83192411778853));
#14414=CARTESIAN_POINT('Ctrl Pts',(-0.454318949508754,0.0194457328714482,
2.81544408284231));
#14415=CARTESIAN_POINT('Ctrl Pts',(-0.574388741029553,0.0112334439036321,
2.79100586565238));
#14416=CARTESIAN_POINT('Ctrl Pts',(-0.62915108024243,0.007487921000048,
2.77985989860636));
#14417=CARTESIAN_POINT('Ctrl Pts',(-0.68357621353279,0.00374226744711259,
2.7670592115551));
#14418=CARTESIAN_POINT('Ctrl Pts',(-0.737555719985232,-3.51596576807223E-6,
2.75259542039799));
#14419=CARTESIAN_POINT('Ctrl Pts',(-0.855910739555236,-0.00821648970844346,
2.72088223148684));
#14420=CARTESIAN_POINT('Ctrl Pts',(-0.972121952743627,-0.016430087747433,
2.68117054902539));
#14421=CARTESIAN_POINT('Ctrl Pts',(-1.08524943432292,-0.0246443017617273,
2.63412173290116));
#14422=CARTESIAN_POINT('Ctrl Pts',(-1.13684304884904,-0.0283905266893244,
2.61266436065937));
#14423=CARTESIAN_POINT('Ctrl Pts',(-1.1877955424641,-0.0321368797375203,
2.58968156208569));
#14424=CARTESIAN_POINT('Ctrl Pts',(-1.23801956154725,-0.0358833601169834,
2.56523916887831));
#14425=CARTESIAN_POINT('Ctrl Pts',(-1.36006367903396,-0.0449872888733795,
2.50584427450875));
#14426=CARTESIAN_POINT('Ctrl Pts',(-1.47787419080016,-0.0540901924371456,
2.43780365338667));
#14427=CARTESIAN_POINT('Ctrl Pts',(-1.59039424635548,-0.0631922589418942,
2.36191920832476));
#14428=CARTESIAN_POINT('Ctrl Pts',(-1.70277447939221,-0.0722830148064472,
2.28612906071213));
#14429=CARTESIAN_POINT('Ctrl Pts',(-1.80987841761559,-0.0813729356910015,
2.20251382274258));
#14430=CARTESIAN_POINT('Ctrl Pts',(-1.91062667852844,-0.0904622090286987,
2.11182884014686));
#14431=CARTESIAN_POINT('Ctrl Pts',(-1.9740717901352,-0.0961860791591553,
2.05472096761674));
#14432=CARTESIAN_POINT('Ctrl Pts',(-2.03499584355038,-0.10190969249116,
1.99480860783181));
#14433=CARTESIAN_POINT('Ctrl Pts',(-2.09312110392871,-0.107633095833601,
1.93227353006217));
#14434=CARTESIAN_POINT('Ctrl Pts',(-2.17725469900751,-0.115917454409398,
1.84175693061733));
#14435=CARTESIAN_POINT('Ctrl Pts',(-2.25553549330611,-0.124202880489431,
1.74572510198876));
#14436=CARTESIAN_POINT('Ctrl Pts',(-2.32700347370338,-0.13248905593599,
1.64486162842615));
#14437=CARTESIAN_POINT('Ctrl Pts',(-2.34166723806075,-0.134189209256356,
1.6241665115309));
#14438=CARTESIAN_POINT('Ctrl Pts',(-2.35604431386819,-0.135889394124023,
1.60326811487315));
#14439=CARTESIAN_POINT('Ctrl Pts',(-2.37012661068211,-0.137589607790991,
1.58217252837426));
#14440=CARTESIAN_POINT('Ctrl Pts',(-2.43887420373001,-0.145889787713038,
1.47918714077051));
#14441=CARTESIAN_POINT('Ctrl Pts',(-2.50059269511661,-0.154190653991916,
1.37150029709983));
#14442=CARTESIAN_POINT('Ctrl Pts',(-2.55500200152593,-0.162491886908244,
1.26025962660104));
#14443=CARTESIAN_POINT('Ctrl Pts',(-2.59191434546933,-0.168123606641198,
1.18479176713129));
#14444=CARTESIAN_POINT('Ctrl Pts',(-2.62546356838125,-0.173755495120222,
1.10768889203951));
#14445=CARTESIAN_POINT('Ctrl Pts',(-2.65557518457384,-0.17938745251458,
1.02931353467584));
#14446=CARTESIAN_POINT('Ctrl Pts',(-2.70517097227751,-0.188663652154619,
0.900224230397167));
#14447=CARTESIAN_POINT('Ctrl Pts',(-2.74548922999383,-0.197938556591528,
0.76757664521583));
#14448=CARTESIAN_POINT('Ctrl Pts',(-2.77623467558263,-0.207212589244025,
0.632745539129348));
#14449=CARTESIAN_POINT('Ctrl Pts',(-2.80666391168401,-0.216391240708993,
0.499301138427257));
#14450=CARTESIAN_POINT('Ctrl Pts',(-2.82771643357988,-0.225569038229503,
0.363716648488724));
#14451=CARTESIAN_POINT('Ctrl Pts',(-2.83905719972122,-0.234746392293966,
0.227314229871604));
#14452=CARTESIAN_POINT('Ctrl Pts',(-2.84580784954219,-0.240209259863949,
0.146119983262331));
#14453=CARTESIAN_POINT('Ctrl Pts',(-2.84911640035801,-0.24567197030472,
0.064635807190785));
#14454=CARTESIAN_POINT('Ctrl Pts',(-2.84890338395658,-0.251134610194849,
-0.0168585082596733));
#14455=CARTESIAN_POINT('Ctrl Pts',(-2.84859095134652,-0.259146701410729,
-0.136386777026674));
#14456=CARTESIAN_POINT('Ctrl Pts',(-2.84069830829409,-0.267160119774128,
-0.25591825162007));
#14457=CARTESIAN_POINT('Ctrl Pts',(-2.82499127124688,-0.275174317819118,
-0.374425444279389));
#14458=CARTESIAN_POINT('Ctrl Pts',(-2.80820184658356,-0.283740782258516,
-0.501099085987492));
#14459=CARTESIAN_POINT('Ctrl Pts',(-2.78248344796085,-0.292308137539294,
-0.62660131446913));
#14460=CARTESIAN_POINT('Ctrl Pts',(-2.74843102357668,-0.300875715037838,
-0.749793091323411));
#14461=CARTESIAN_POINT('Ctrl Pts',(-2.7192635507982,-0.308214240502195,
-0.85531253268221));
#14462=CARTESIAN_POINT('Ctrl Pts',(-2.68398275963749,-0.315552929001334,
-0.959136584134086));
#14463=CARTESIAN_POINT('Ctrl Pts',(-2.64299019944675,-0.322891360356581,
-1.06056200859463));
#14464=CARTESIAN_POINT('Ctrl Pts',(-2.58928984766141,-0.332504722964227,
-1.19342955695376));
#14465=CARTESIAN_POINT('Ctrl Pts',(-2.52573563654052,-0.34211651623184,
-1.32233107103795));
#14466=CARTESIAN_POINT('Ctrl Pts',(-2.45307990206561,-0.35172744735852,
-1.44588164571447));
#14467=CARTESIAN_POINT('Ctrl Pts',(-2.38190226984351,-0.361142854497278,
-1.56691871771862));
#14468=CARTESIAN_POINT('Ctrl Pts',(-2.30198893075688,-0.370557434216932,
-1.6828213822311));
#14469=CARTESIAN_POINT('Ctrl Pts',(-2.21400728279147,-0.379971851427205,
-1.79225939560688));
#14470=CARTESIAN_POINT('Ctrl Pts',(-2.1683256449433,-0.384859984435583,
-1.84908156033628));
#14471=CARTESIAN_POINT('Ctrl Pts',(-2.12046830077378,-0.389748073633526,
-1.90416037877037));
#14472=CARTESIAN_POINT('Ctrl Pts',(-2.07052526111232,-0.394636212091378,
-1.95730518181801));
#14473=CARTESIAN_POINT('Ctrl Pts',(-2.00881800212756,-0.400675764906277,
-2.02296838829451));
#14474=CARTESIAN_POINT('Ctrl Pts',(-1.94394844543176,-0.406716201619121,
-2.08565406472235));
#14475=CARTESIAN_POINT('Ctrl Pts',(-1.8761293000041,-0.412757196014427,
-2.14497294477118));
#14476=CARTESIAN_POINT('Ctrl Pts',(-1.77418651530985,-0.421837755598251,
-2.23413850088353));
#14477=CARTESIAN_POINT('Ctrl Pts',(-1.66557812957501,-0.430919575254045,
-2.31569450072344));
#14478=CARTESIAN_POINT('Ctrl Pts',(-1.55171138002138,-0.440001547039586,
-2.38910295251116));
#14479=CARTESIAN_POINT('Ctrl Pts',(-1.44140473304468,-0.448799566299178,
-2.46021625124145));
#14480=CARTESIAN_POINT('Ctrl Pts',(-1.3261645781001,-0.457597728324383,
-2.52368334697871));
#14481=CARTESIAN_POINT('Ctrl Pts',(-1.20728772228421,-0.466395025878857,
-2.57905840053748));
#14482=CARTESIAN_POINT('Ctrl Pts',(-1.06924625101902,-0.476610571110452,
-2.64336068891968));
#14483=CARTESIAN_POINT('Ctrl Pts',(-0.926118773149324,-0.486824213024927,
-2.69684664251162));
#14484=CARTESIAN_POINT('Ctrl Pts',(-0.77969440642078,-0.497037072922188,
-2.73883496415487));
#14485=CARTESIAN_POINT('Ctrl Pts',(-0.638052790054798,-0.506916343810545,
-2.7794517950753));
#14486=CARTESIAN_POINT('Ctrl Pts',(-0.49332491118727,-0.516794882934398,
-2.80931002663451));
#14487=CARTESIAN_POINT('Ctrl Pts',(-0.347125828863604,-0.526673705266467,
-2.82774527917647));
#14488=CARTESIAN_POINT('Ctrl Pts',(-0.290572441659506,-0.530495075794835,
-2.83487648655917));
#14489=CARTESIAN_POINT('Ctrl Pts',(-0.23379896130483,-0.53431648870055,
-2.84029790415576));
#14490=CARTESIAN_POINT('Ctrl Pts',(-0.176899268891918,-0.538138002732039,
-2.84396897512448));
#14491=CARTESIAN_POINT('Ctrl Pts',(-0.116352231391689,-0.542204480836932,
-2.84787536656851));
#14492=CARTESIAN_POINT('Ctrl Pts',(-0.0556864187648436,-0.546271383042092,
-2.84979803401917));
#14493=CARTESIAN_POINT('Ctrl Pts',(0.00497365610244438,-0.550338591071923,
-2.8496921406586));
#14494=CARTESIAN_POINT('Ctrl Pts',(0.154530000355481,-0.560366220704572,
-2.84943106244659));
#14495=CARTESIAN_POINT('Ctrl Pts',(0.304050612630736,-0.570395709324061,
-2.83683559990313));
#14496=CARTESIAN_POINT('Ctrl Pts',(0.451675731743237,-0.5804252843707,-2.81261256222691));
#14497=CARTESIAN_POINT('Ctrl Pts',(0.596287470173571,-0.590250131875864,
-2.78888397450767));
#14498=CARTESIAN_POINT('Ctrl Pts',(0.739079140294107,-0.600075062315811,
-2.75399829388592));
#14499=CARTESIAN_POINT('Ctrl Pts',(0.878322966205294,-0.609898409476766,
-2.70866393343392));
#14500=CARTESIAN_POINT('Ctrl Pts',(1.04784464245577,-0.621857792711305,
-2.65347185058733));
#14501=CARTESIAN_POINT('Ctrl Pts',(1.21239860104531,-0.633814470368098,
-2.58270958152775));
#14502=CARTESIAN_POINT('Ctrl Pts',(1.36904374063119,-0.645770674535305,
-2.49743826863348));
#14503=CARTESIAN_POINT('Ctrl Pts',(1.51022988132689,-0.656546944569603,
-2.42058221289232));
#14504=CARTESIAN_POINT('Ctrl Pts',(1.64499180429864,-0.667322829958374,
-2.33193849640115));
#14505=CARTESIAN_POINT('Ctrl Pts',(1.7711385373037,-0.678099965020317,-2.23225318102518));
#14506=CARTESIAN_POINT('Ctrl Pts',(1.78495081516552,-0.67927999386834,-2.22133826280323));
#14507=CARTESIAN_POINT('Ctrl Pts',(1.79865976111333,-0.680460037698545,
-2.21029094308228));
#14508=CARTESIAN_POINT('Ctrl Pts',(1.81226246383145,-0.681640098656313,
-2.19911218332638));
#14509=CARTESIAN_POINT('Ctrl Pts',(1.83638940132602,-0.683733157481302,
-2.17928456204503));
#14510=CARTESIAN_POINT('Ctrl Pts',(1.86017575754718,-0.685826322908651,
-2.15904864358979));
#14511=CARTESIAN_POINT('Ctrl Pts',(1.88360520990837,-0.687919577979938,
-2.13841094879892));
#14512=CARTESIAN_POINT('Ctrl Pts',(2.01767668833799,-0.699897911822797,
-2.0203148785478));
#14513=CARTESIAN_POINT('Ctrl Pts',(2.14005752488522,-0.711879181080226,
-1.8890612688117));
#14514=CARTESIAN_POINT('Ctrl Pts',(2.24922740729515,-0.7238602080859,-1.74760001821103));
#14515=CARTESIAN_POINT('Ctrl Pts',(2.33895996050149,-0.733708053659428,
-1.63132546596324));
#14516=CARTESIAN_POINT('Ctrl Pts',(2.41976767616667,-0.743555735565897,
-1.50815535967203));
#14517=CARTESIAN_POINT('Ctrl Pts',(2.49083272407377,-0.753401489190834,
-1.37973020927764));
#14518=CARTESIAN_POINT('Ctrl Pts',(2.58692232024631,-0.766714285251585,
-1.20608196441995));
#14519=CARTESIAN_POINT('Ctrl Pts',(2.66539065768445,-0.780023697310082,
-1.02249109650153));
#14520=CARTESIAN_POINT('Ctrl Pts',(2.72408373297952,-0.793333409033395,
-0.832806588169003));
#14521=CARTESIAN_POINT('Ctrl Pts',(2.77083752169619,-0.803935672531488,
-0.681707512497436));
#14522=CARTESIAN_POINT('Ctrl Pts',(2.80504246184954,-0.81453812617926,-0.526742078154303));
#14523=CARTESIAN_POINT('Ctrl Pts',(2.8255909834669,-0.825142631936016,-0.369870509681839));
#14524=CARTESIAN_POINT('Ctrl Pts',(2.82582273756608,-0.825262233614654,
-0.368101252033223));
#14525=CARTESIAN_POINT('Ctrl Pts',(2.82605275056068,-0.825381835575542,
-0.366331781103057));
#14526=CARTESIAN_POINT('Ctrl Pts',(2.82628102101889,-0.825501437815763,
-0.364562099745109));
#14527=CARTESIAN_POINT('Ctrl Pts',(2.85228039059975,-0.839123799949733,
-0.163000320674225));
#14528=CARTESIAN_POINT('Ctrl Pts',(2.85567668810618,-0.852749785743964,
0.0412871256586262));
#14529=CARTESIAN_POINT('Ctrl Pts',(2.83767946395795,-0.866375084534093,
0.243678475560316));
#14530=CARTESIAN_POINT('Ctrl Pts',(2.82423649436951,-0.876552458320218,
0.39485405348747));
#14531=CARTESIAN_POINT('Ctrl Pts',(2.79885689994874,-0.886729448806458,
0.544972862464313));
#14532=CARTESIAN_POINT('Ctrl Pts',(2.76203586844939,-0.896904259550461,
0.692125424989613));
#14533=CARTESIAN_POINT('Ctrl Pts',(2.71744107462166,-0.909227205673603,
0.870345260768906));
#14534=CARTESIAN_POINT('Ctrl Pts',(2.65597926441388,-0.921547418985483,
1.04453367619778));
#14535=CARTESIAN_POINT('Ctrl Pts',(2.57838960400743,-0.933868114421141,
1.21118089962741));
#14536=CARTESIAN_POINT('Ctrl Pts',(2.51706685619316,-0.943605737902665,
1.34289001657406));
#14537=CARTESIAN_POINT('Ctrl Pts',(2.44567101895833,-0.95334366254192,1.46988763932027));
#14538=CARTESIAN_POINT('Ctrl Pts',(2.36458933503997,-0.963083475516264,
1.59043615941138));
#14539=CARTESIAN_POINT('Ctrl Pts',(2.34915516664531,-0.964937481332544,
1.61338297142735));
#14540=CARTESIAN_POINT('Ctrl Pts',(2.33337009128119,-0.966791555571495,
1.63609610498031));
#14541=CARTESIAN_POINT('Ctrl Pts',(2.31724389399609,-0.968645709180412,
1.65856831625786));
#14542=CARTESIAN_POINT('Ctrl Pts',(2.22206520595145,-0.979589138980383,
1.79120191542856));
#14543=CARTESIAN_POINT('Ctrl Pts',(2.11514122746783,-0.990534146427008,
1.91525839371467));
#14544=CARTESIAN_POINT('Ctrl Pts',(1.99849993464102,-1.0014788962736,2.02939768246979));
#14545=CARTESIAN_POINT('Ctrl Pts',(1.87549830855913,-1.0130204524032,2.14976087269569));
#14546=CARTESIAN_POINT('Ctrl Pts',(1.74169002021321,-1.02456172207351,2.25909682066194));
#14547=CARTESIAN_POINT('Ctrl Pts',(1.59940027188827,-1.03610055314691,2.3558139759935));
#14548=CARTESIAN_POINT('Ctrl Pts',(1.58169941761635,-1.03753598450934,2.36784559662867));
#14549=CARTESIAN_POINT('Ctrl Pts',(1.56386725431272,-1.03897137813357,2.3796819008649));
#14550=CARTESIAN_POINT('Ctrl Pts',(1.54590821413885,-1.04040672987643,2.39131979215231));
#14551=CARTESIAN_POINT('Ctrl Pts',(1.41850062270793,-1.05058960750483,2.47388298505734));
#14552=CARTESIAN_POINT('Ctrl Pts',(1.2845210901381,-1.06077094234822,2.54657562083443));
#14553=CARTESIAN_POINT('Ctrl Pts',(1.14562765742176,-1.07095249073693,2.60814967754909));
#14554=CARTESIAN_POINT('Ctrl Pts',(1.01052845018237,-1.08085590437486,2.66804168313909));
#14555=CARTESIAN_POINT('Ctrl Pts',(0.870781356165271,-1.09075952005037,
2.71741367426934));
#14556=CARTESIAN_POINT('Ctrl Pts',(0.727942869331522,-1.10066495405409,
2.75515317742913));
#14557=CARTESIAN_POINT('Ctrl Pts',(0.672745192890889,-1.10449275252256,
2.76973701215477));
#14558=CARTESIAN_POINT('Ctrl Pts',(0.617086111586118,-1.10832082252452,
2.78258418807595));
#14559=CARTESIAN_POINT('Ctrl Pts',(0.561075206954555,-1.11214925733085,
2.79370443055281));
#14560=CARTESIAN_POINT('Ctrl Pts',(0.415939980854654,-1.12206948188143,
2.82251915719901));
#14561=CARTESIAN_POINT('Ctrl Pts',(0.268591246834638,-1.1319903866323,2.83971425995812));
#14562=CARTESIAN_POINT('Ctrl Pts',(0.12079118009236,-1.14191092298971,2.84554363412139));
#14563=CARTESIAN_POINT('Ctrl Pts',(-0.032618438032068,-1.15220797987016,
2.85159425428688));
#14564=CARTESIAN_POINT('Ctrl Pts',(-0.186515561471283,-1.16250463986278,
2.84540020170277));
#14565=CARTESIAN_POINT('Ctrl Pts',(-0.338946955042084,-1.17279973039116,
2.82719276804528));
#14566=CARTESIAN_POINT('Ctrl Pts',(-0.393778617605422,-1.17650301563108,
2.82064330447963));
#14567=CARTESIAN_POINT('Ctrl Pts',(-0.448420685577804,-1.18020609779181,
2.81253889014373));
#14568=CARTESIAN_POINT('Ctrl Pts',(-0.502782257634685,-1.18390892229605,
2.80288865320055));
#14569=CARTESIAN_POINT('Ctrl Pts',(-0.637274623859498,-1.19306983524332,
2.77901364090767));
#14570=CARTESIAN_POINT('Ctrl Pts',(-0.770213396999383,-1.20222989352261,
2.74564308769741));
#14571=CARTESIAN_POINT('Ctrl Pts',(-0.900056879936483,-1.21139019744609,
2.70289282289534));
#14572=CARTESIAN_POINT('Ctrl Pts',(-1.02694447851203,-1.22034196722906,
2.66111576703933));
#14573=CARTESIAN_POINT('Ctrl Pts',(-1.15087493148394,-1.22929397159932,
2.61038149471995));
#14574=CARTESIAN_POINT('Ctrl Pts',(-1.27041542598044,-1.23824723742104,
2.55084583424531));
#14575=CARTESIAN_POINT('Ctrl Pts',(-1.34787274881595,-1.24404858535845,
2.51226917540653));
#14576=CARTESIAN_POINT('Ctrl Pts',(-1.42348713502069,-1.24985046291713,
2.46999825131315));
#14577=CARTESIAN_POINT('Ctrl Pts',(-1.49698933741267,-1.25565314945133,
2.42431798977058));
#14578=CARTESIAN_POINT('Ctrl Pts',(-1.61624974890631,-1.26506825214644,
2.35019984621277));
#14579=CARTESIAN_POINT('Ctrl Pts',(-1.72987865084394,-1.27448345518868,
2.26715757146334));
#14580=CARTESIAN_POINT('Ctrl Pts',(-1.8369037071566,-1.28389814149844,2.17633379704892));
#14581=CARTESIAN_POINT('Ctrl Pts',(-1.94676850078249,-1.29356263133018,
2.0831001602152));
#14582=CARTESIAN_POINT('Ctrl Pts',(-2.04967536339833,-1.30322657664433,
1.98166583179054));
#14583=CARTESIAN_POINT('Ctrl Pts',(-2.14454649169789,-1.31288930992677,
1.87321917481648));
#14584=CARTESIAN_POINT('Ctrl Pts',(-2.19207519461938,-1.31773016285876,
1.81888937991962));
#14585=CARTESIAN_POINT('Ctrl Pts',(-2.2375865690511,-1.32257071159175,1.76279894915519));
#14586=CARTESIAN_POINT('Ctrl Pts',(-2.2809414956653,-1.32741087219403,1.70509395756389));
#14587=CARTESIAN_POINT('Ctrl Pts',(-2.35806048512942,-1.33602046569683,
1.60244932208436));
#14588=CARTESIAN_POINT('Ctrl Pts',(-2.42843033480345,-1.34462973490771,
1.4945890168124));
#14589=CARTESIAN_POINT('Ctrl Pts',(-2.49113853055435,-1.35323935515332,
1.38244863236214));
#14590=CARTESIAN_POINT('Ctrl Pts',(-2.54598462287356,-1.3607695355575,1.28436796197092));
#14591=CARTESIAN_POINT('Ctrl Pts',(-2.5949698842659,-1.36829998449169,1.18301421805579));
#14592=CARTESIAN_POINT('Ctrl Pts',(-2.63750948583029,-1.37583115378905,
1.07903361952129));
#14593=CARTESIAN_POINT('Ctrl Pts',(-2.68142316890915,-1.38360558912872,
0.971694319610797));
#14594=CARTESIAN_POINT('Ctrl Pts',(-2.71846769641451,-1.39138079212042,
0.861556290119179));
#14595=CARTESIAN_POINT('Ctrl Pts',(-2.74861153842052,-1.39915725981108,
0.749579659818414));
#14596=CARTESIAN_POINT('Ctrl Pts',(-2.78412055464879,-1.40831782790891,
0.617672785381378));
#14597=CARTESIAN_POINT('Ctrl Pts',(-2.81005394236977,-1.41747805955768,
0.483246619510076));
#14598=CARTESIAN_POINT('Ctrl Pts',(-2.82643013810069,-1.42663764140704,
0.347667528530173));
#14599=CARTESIAN_POINT('Ctrl Pts',(-2.84308692979975,-1.43595416701665,
0.209765373823006));
#14600=CARTESIAN_POINT('Ctrl Pts',(-2.84985638294299,-1.44527002036825,
0.0706691911022305));
#14601=CARTESIAN_POINT('Ctrl Pts',(-2.84670661998034,-1.45458487172665,
-0.0681974790284871));
#14602=CARTESIAN_POINT('Ctrl Pts',(-2.84486611926434,-1.46002781800478,
-0.149341428219176));
#14603=CARTESIAN_POINT('Ctrl Pts',(-2.83963781638863,-1.46547042216091,
-0.230407182515753));
#14604=CARTESIAN_POINT('Ctrl Pts',(-2.8310071078325,-1.47091261840812,-0.311110263182307));
#14605=CARTESIAN_POINT('Ctrl Pts',(-2.81781371033578,-1.47923187260117,
-0.434477633951345));
#14606=CARTESIAN_POINT('Ctrl Pts',(-2.79665378128776,-1.48755127053128,
-0.557093791266127));
#14607=CARTESIAN_POINT('Ctrl Pts',(-2.76747059455719,-1.49587114828328,
-0.677766985411362));
#14608=CARTESIAN_POINT('Ctrl Pts',(-2.74695702916998,-1.50171939089827,
-0.762591082294128));
#14609=CARTESIAN_POINT('Ctrl Pts',(-2.72248022415427,-1.50756787059436,
-0.846454899621325));
#14610=CARTESIAN_POINT('Ctrl Pts',(-2.69403586235103,-1.51341670409936,
-0.928945999604021));
#14611=CARTESIAN_POINT('Ctrl Pts',(-2.65364415779899,-1.52172219383198,
-1.04608542293585));
#14612=CARTESIAN_POINT('Ctrl Pts',(-2.60525022569129,-1.53002839701002,
-1.16045536951902));
#14613=CARTESIAN_POINT('Ctrl Pts',(-2.54960516799807,-1.53833564787641,
-1.27114014825599));
#14614=CARTESIAN_POINT('Ctrl Pts',(-2.53994671480788,-1.53977755838847,
-1.29035198482539));
#14615=CARTESIAN_POINT('Ctrl Pts',(-2.53006991307008,-1.54121950046469,
-1.30945286158362));
#14616=CARTESIAN_POINT('Ctrl Pts',(-2.51997882226938,-1.5426614758529,-1.32843807863483));
#14617=CARTESIAN_POINT('Ctrl Pts',(-2.45657270677688,-1.55172194907707,
-1.44772933156009));
#14618=CARTESIAN_POINT('Ctrl Pts',(-2.38470081591898,-1.56078173197691,
-1.56247422468651));
#14619=CARTESIAN_POINT('Ctrl Pts',(-2.3052368403023,-1.56984075937861,-1.67169370439398));
#14620=CARTESIAN_POINT('Ctrl Pts',(-2.22510581752997,-1.57897583128243,
-1.78183000889803));
#14621=CARTESIAN_POINT('Ctrl Pts',(-2.13725395829225,-1.58811013495105,
-1.88634876066361));
#14622=CARTESIAN_POINT('Ctrl Pts',(-2.04253202532631,-1.59724360355553,
-1.98421985142671));
#14623=CARTESIAN_POINT('Ctrl Pts',(-1.98317053855799,-1.60296747614488,
-2.0455548904976));
#14624=CARTESIAN_POINT('Ctrl Pts',(-1.92111002239413,-1.60869102076865,
-2.10427853314291));
#14625=CARTESIAN_POINT('Ctrl Pts',(-1.85655299640856,-1.61441422097834,
-2.16012933435915));
#14626=CARTESIAN_POINT('Ctrl Pts',(-1.76394106594421,-1.62262458401413,
-2.2402515277169));
#14627=CARTESIAN_POINT('Ctrl Pts',(-1.66613907414915,-1.63083553082874,
-2.31449904720288));
#14628=CARTESIAN_POINT('Ctrl Pts',(-1.56387127587846,-1.63904709023554,
-2.38197566886126));
#14629=CARTESIAN_POINT('Ctrl Pts',(-1.51423913488985,-1.64303228675983,
-2.41472311484342));
#14630=CARTESIAN_POINT('Ctrl Pts',(-1.46355574560736,-1.64701762756862,
-2.44587630950781));
#14631=CARTESIAN_POINT('Ctrl Pts',(-1.41190681906569,-1.65100311595549,
-2.47533616148238));
#14632=CARTESIAN_POINT('Ctrl Pts',(-1.30550422906709,-1.65921366969139,
-2.53602676554636));
#14633=CARTESIAN_POINT('Ctrl Pts',(-1.1950027195626,-1.66742484975796,-2.58952751654282));
#14634=CARTESIAN_POINT('Ctrl Pts',(-1.08153463719784,-1.67563668495174,
-2.63564802546423));
#14635=CARTESIAN_POINT('Ctrl Pts',(-1.03304098215896,-1.67914623490468,
-2.65535887280774));
#14636=CARTESIAN_POINT('Ctrl Pts',(-0.984005717021573,-1.68265590451736,
-2.67372232411164));
#14637=CARTESIAN_POINT('Ctrl Pts',(-0.934517956492218,-1.68616569603766,
-2.69072631614391));
#14638=CARTESIAN_POINT('Ctrl Pts',(-0.806271691038139,-1.69526123097774,
-2.73479172651251));
#14639=CARTESIAN_POINT('Ctrl Pts',(-0.674924695864088,-1.7043557744404,
-2.7697542564575));
#14640=CARTESIAN_POINT('Ctrl Pts',(-0.541788878943015,-1.71344948581134,
-2.79544280040553));
#14641=CARTESIAN_POINT('Ctrl Pts',(-0.408659211874132,-1.72254277712265,
-2.82113015774013));
#14642=CARTESIAN_POINT('Ctrl Pts',(-0.273739637134264,-1.73163523641909,
-2.83754458164282));
#14643=CARTESIAN_POINT('Ctrl Pts',(-0.138329457050682,-1.74072702306423,
-2.84446539794242));
#14644=CARTESIAN_POINT('Ctrl Pts',(-0.0529910806746092,-1.74645686043817,
-2.84882704361663));
#14645=CARTESIAN_POINT('Ctrl Pts',(0.0325423380463692,-1.75218643064925,
-2.8494170305828));
#14646=CARTESIAN_POINT('Ctrl Pts',(0.117944702086942,-1.75791577358787,
-2.84616945617145));
#14647=CARTESIAN_POINT('Ctrl Pts',(0.241332803706742,-1.76619344548451,
-2.84147740758488));
#14648=CARTESIAN_POINT('Ctrl Pts',(0.364474224217159,-1.77447212945813,
-2.82876802081294));
#14649=CARTESIAN_POINT('Ctrl Pts',(0.486208475639264,-1.78275154654318,
-2.80785133344645));
#14650=CARTESIAN_POINT('Ctrl Pts',(0.514819391444495,-1.78469743853635,
-2.8029353334368));
#14651=CARTESIAN_POINT('Ctrl Pts',(0.543352572900193,-1.78664337102512,
-2.79756620469295));
#14652=CARTESIAN_POINT('Ctrl Pts',(0.571792972249852,-1.78858934038785,
-2.79174190249468));
#14653=CARTESIAN_POINT('Ctrl Pts',(0.692971647225559,-1.7968807144301,-2.76692575225826));
#14654=CARTESIAN_POINT('Ctrl Pts',(0.812464588866411,-1.80517275789546,
-2.73384222121513));
#14655=CARTESIAN_POINT('Ctrl Pts',(0.929267711739225,-1.8134651906415,-2.69310782065252));
#14656=CARTESIAN_POINT('Ctrl Pts',(1.00534859807176,-1.81886654993442,-2.66657506003102));
#14657=CARTESIAN_POINT('Ctrl Pts',(1.08028852426493,-1.8242680743874,-2.63679735865193));
#14658=CARTESIAN_POINT('Ctrl Pts',(1.15381545442221,-1.82966968658238,-2.603955633288));
#14659=CARTESIAN_POINT('Ctrl Pts',(1.27996989407616,-1.83893754746313,-2.54760717087168));
#14660=CARTESIAN_POINT('Ctrl Pts',(1.40206986362378,-1.84820414389981,-2.48219900974871));
#14661=CARTESIAN_POINT('Ctrl Pts',(1.51894129549226,-1.85746987740176,-2.40849865032819));
#14662=CARTESIAN_POINT('Ctrl Pts',(1.63470780780595,-1.8666480113084,-2.33549506484991));
#14663=CARTESIAN_POINT('Ctrl Pts',(1.74534520783587,-1.87582529851979,-2.25435458956647));
#14664=CARTESIAN_POINT('Ctrl Pts',(1.84968554364318,-1.88500212926488,-2.16578098172825));
#14665=CARTESIAN_POINT('Ctrl Pts',(1.91189974797703,-1.89047392709545,-2.11296788223038));
#14666=CARTESIAN_POINT('Ctrl Pts',(1.97187457949454,-1.89594556263917,-2.05751133736491));
#14667=CARTESIAN_POINT('Ctrl Pts',(2.02935554639636,-1.90141711862002,-1.99955491386437));
#14668=CARTESIAN_POINT('Ctrl Pts',(2.11603817247803,-1.90966835144954,-1.91215528824726));
#14669=CARTESIAN_POINT('Ctrl Pts',(2.19703442575146,-1.91792098236696,-1.81907843166739));
#14670=CARTESIAN_POINT('Ctrl Pts',(2.27137118380573,-1.92617442917523,-1.7209424871885));
#14671=CARTESIAN_POINT('Ctrl Pts',(2.34817371186233,-1.93470164500556,-1.61955134737449));
#14672=CARTESIAN_POINT('Ctrl Pts',(2.41786670209158,-1.94322973175108,-1.51276058838507));
#14673=CARTESIAN_POINT('Ctrl Pts',(2.48007992947221,-1.95175804733692,-1.40178648915373));
#14674=CARTESIAN_POINT('Ctrl Pts',(2.53215578122658,-1.95889671087941,-1.3088951381748));
#14675=CARTESIAN_POINT('Ctrl Pts',(2.57899153730472,-1.96603553476112,-1.21307363921052));
#14676=CARTESIAN_POINT('Ctrl Pts',(2.62039639755441,-1.97317414241128,-1.11504501496294));
#14677=CARTESIAN_POINT('Ctrl Pts',(2.67503572119203,-1.98259450251797,-0.985682961964462));
#14678=CARTESIAN_POINT('Ctrl Pts',(2.72028312241804,-1.99201334903906,-0.85234232372255));
#14679=CARTESIAN_POINT('Ctrl Pts',(2.75573316399703,-2.00143131453587,-0.716444766366111));
#14680=CARTESIAN_POINT('Ctrl Pts',(2.79050233332678,-2.01066839360589,-0.583157329376883));
#14681=CARTESIAN_POINT('Ctrl Pts',(2.81584707486254,-2.01990462516945,-0.447409014739265));
#14682=CARTESIAN_POINT('Ctrl Pts',(2.8313366954026,-2.02914060603565,-0.310532368306937));
#14683=CARTESIAN_POINT('Ctrl Pts',(2.84015746635835,-2.03440015849283,-0.232586136877494));
#14684=CARTESIAN_POINT('Ctrl Pts',(2.84578143549661,-2.03965962965174,-0.154273939294073));
#14685=CARTESIAN_POINT('Ctrl Pts',(2.84812148408046,-2.04491912972532,-0.0758428334344391));
#14686=CARTESIAN_POINT('Ctrl Pts',(2.85091497943733,-2.05119779809844,0.0177863892939412));
#14687=CARTESIAN_POINT('Ctrl Pts',(2.84902594284215,-2.05747737660946,0.111557393492299));
#14688=CARTESIAN_POINT('Ctrl Pts',(2.8423143279138,-2.06375753276342,0.204986229314948));
#14689=CARTESIAN_POINT('Ctrl Pts',(2.83287159820045,-2.07259323292689,0.336433467204058));
#14690=CARTESIAN_POINT('Ctrl Pts',(2.813880666638,-2.08143007649653,0.467202554864027));
#14691=CARTESIAN_POINT('Ctrl Pts',(2.78589826341793,-2.09026713750293,0.596029432374906));
#14692=CARTESIAN_POINT('Ctrl Pts',(2.75802274342066,-2.09907044395463,0.72436423521504));
#14693=CARTESIAN_POINT('Ctrl Pts',(2.72122485788936,-2.10787396618517,0.850770535434859));
#14694=CARTESIAN_POINT('Ctrl Pts',(2.67610312119081,-2.11667678879524,0.974016832256147));
#14695=CARTESIAN_POINT('Ctrl Pts',(-2.097235989958,2.319248086811,0.5776750355837));
#14696=CARTESIAN_POINT('Ctrl Pts',(-2.235952065827,2.2733869757,0.07406949825217));
#14697=CARTESIAN_POINT('Ctrl Pts',(-2.133884893527,2.181664753478,-1.034686203893));
#14698=CARTESIAN_POINT('Ctrl Pts',(-0.9210292495221,2.044081420145,-2.185735282405));
#14699=CARTESIAN_POINT('Ctrl Pts',(0.7496331376127,1.906498086811,-2.25015296747));
#14700=CARTESIAN_POINT('Ctrl Pts',(2.047765400978,1.768914753478,-1.196625791736));
#14701=CARTESIAN_POINT('Ctrl Pts',(2.328382246189,1.631331420145,0.4515392303455));
#14702=CARTESIAN_POINT('Ctrl Pts',(1.452032556261,1.493748086811,1.875325701807));
#14703=CARTESIAN_POINT('Ctrl Pts',(-0.1458254019403,1.356164753478,2.367273318177));
#14704=CARTESIAN_POINT('Ctrl Pts',(-1.671223522139,1.218581420145,1.682931733308));
#14705=CARTESIAN_POINT('Ctrl Pts',(-2.366197443666,1.080998086811,0.1623484463472));
#14706=CARTESIAN_POINT('Ctrl Pts',(-1.885417534126,0.9434147534781,-1.43890517495));
#14707=CARTESIAN_POINT('Ctrl Pts',(-0.4677813480371,0.8058314201447,-2.325172676827));
#14708=CARTESIAN_POINT('Ctrl Pts',(1.182293478365,0.6682480868114,-2.056071375655));
#14709=CARTESIAN_POINT('Ctrl Pts',(2.244891504223,0.5306647534781,-0.7653166040083));
#14710=CARTESIAN_POINT('Ctrl Pts',(2.192012109843,0.3930814201447,0.9057208622855));
#14711=CARTESIAN_POINT('Ctrl Pts',(1.049930850427,0.2554980868114,2.12670933121));
#14712=CARTESIAN_POINT('Ctrl Pts',(-0.6138567605814,0.1179147534781,2.290944619059));
#14713=CARTESIAN_POINT('Ctrl Pts',(-1.972621454292,-0.01966857985527,1.31681888208));
#14714=CARTESIAN_POINT('Ctrl Pts',(-2.35119860367,-0.1572519131886,-0.3116287794445));
#14715=CARTESIAN_POINT('Ctrl Pts',(-1.561474769393,-0.2948352465219,-1.785229373121));
#14716=CARTESIAN_POINT('Ctrl Pts',(0.004139500834496,-0.4324185798553,-2.371756782494));
#14717=CARTESIAN_POINT('Ctrl Pts',(1.56769686923,-0.5700019131886,-1.779767932299));
#14718=CARTESIAN_POINT('Ctrl Pts',(2.352272068769,-0.7075852465219,-0.3034196680806));
#14719=CARTESIAN_POINT('Ctrl Pts',(1.968012873411,-0.8451685798553,1.323696600635));
#14720=CARTESIAN_POINT('Ctrl Pts',(0.6058561589209,-0.9827519131886,2.293073394949));
#14721=CARTESIAN_POINT('Ctrl Pts',(-1.057348156491,-1.120335246522,2.123031532212));
#14722=CARTESIAN_POINT('Ctrl Pts',(-2.195159931747,-1.257918579855,0.8980634200042));
#14723=CARTESIAN_POINT('Ctrl Pts',(-2.242207790093,-1.395501913189,-0.7731466788102));
#14724=CARTESIAN_POINT('Ctrl Pts',(-1.175103962369,-1.533085246522,-2.060191034956));
#14725=CARTESIAN_POINT('Ctrl Pts',(0.4758751430437,-1.670668579855,-2.323506201036));
#14726=CARTESIAN_POINT('Ctrl Pts',(1.890502368917,-1.808251913189,-1.43238765575));
#14727=CARTESIAN_POINT('Ctrl Pts',(2.365341628493,-1.945835246522,0.1708779092467));
#14728=CARTESIAN_POINT('Ctrl Pts',(1.899356541525,-2.037557468744,1.182122100046));
#14729=CARTESIAN_POINT('Ctrl Pts',(1.527422127243,-2.083418579855,1.548899250927));
#14730=CARTESIAN_POINT('Ctrl Pts',(-2.081620410866,2.281336533461,0.5733737884892));
#14731=CARTESIAN_POINT('Ctrl Pts',(-2.219303635942,2.23547542235,0.07351799231108));
#14732=CARTESIAN_POINT('Ctrl Pts',(-2.117996434389,2.143753200128,-1.02698214754));
#14733=CARTESIAN_POINT('Ctrl Pts',(-0.9141714590009,2.006169866795,-2.169460756152));
#14734=CARTESIAN_POINT('Ctrl Pts',(0.7440515265746,1.868586533461,-2.233398800651));
#14735=CARTESIAN_POINT('Ctrl Pts',(2.03251816951,1.731003200128,-1.187715967194));
#14736=CARTESIAN_POINT('Ctrl Pts',(2.311045600577,1.593419866795,0.4481771639882));
#14737=CARTESIAN_POINT('Ctrl Pts',(1.441221026544,1.455836533461,1.861362420153));
#14738=CARTESIAN_POINT('Ctrl Pts',(-0.1447396165978,1.318253200128,2.349647097803));
#14739=CARTESIAN_POINT('Ctrl Pts',(-1.658779942486,1.180669866795,1.670400976771));
#14740=CARTESIAN_POINT('Ctrl Pts',(-2.348579234028,1.043086533461,0.1611396338832));
#14741=CARTESIAN_POINT('Ctrl Pts',(-1.871379110807,0.905503200128,-1.42819138896));
#14742=CARTESIAN_POINT('Ctrl Pts',(-0.4642983462798,0.7679198667947,-2.307859928994));
#14743=CARTESIAN_POINT('Ctrl Pts',(1.17349036922,0.6303365334613,-2.040762299642));
#14744=CARTESIAN_POINT('Ctrl Pts',(2.228176513155,0.492753200128,-0.7596182171705));
#14745=CARTESIAN_POINT('Ctrl Pts',(2.175690847649,0.3551698667947,0.8989770548032));
#14746=CARTESIAN_POINT('Ctrl Pts',(1.042113285635,0.2175865334613,2.110874299803));
#14747=CARTESIAN_POINT('Ctrl Pts',(-0.609286111955,0.080003200128,2.273886726162));
#14748=CARTESIAN_POINT('Ctrl Pts',(-1.957933728882,-0.05758013320533,1.307014125008));
#14749=CARTESIAN_POINT('Ctrl Pts',(-2.333692072247,-0.1951634665387,-0.3093084569456));
#14750=CARTESIAN_POINT('Ctrl Pts',(-1.549848355923,-0.332746799872,-1.771936929824));
#14751=CARTESIAN_POINT('Ctrl Pts',(0.004108678979924,-0.4703301332053,-2.354097179186));
#14752=CARTESIAN_POINT('Ctrl Pts',(1.556024127311,-0.6079134665387,-1.766516153745));
#14753=CARTESIAN_POINT('Ctrl Pts',(2.33475754455,-0.745496799872,-0.3011604689023));
#14754=CARTESIAN_POINT('Ctrl Pts',(1.953359462527,-0.8830801332053,1.313840633513));
#14755=CARTESIAN_POINT('Ctrl Pts',(0.6013450810956,-1.020663466539,2.275999651633));
#14756=CARTESIAN_POINT('Ctrl Pts',(-1.049475363994,-1.158246799872,2.107223884925));
#14757=CARTESIAN_POINT('Ctrl Pts',(-2.178815231532,-1.295830133205,0.8913766282303));
#14758=CARTESIAN_POINT('Ctrl Pts',(-2.225512781398,-1.433413466539,-0.7673899908785));
#14759=CARTESIAN_POINT('Ctrl Pts',(-1.166354384852,-1.570996799872,-2.044851284825));
#14760=CARTESIAN_POINT('Ctrl Pts',(0.4723318765873,-1.708580133205,-2.306205861433));
#14761=CARTESIAN_POINT('Ctrl Pts',(1.876426084985,-1.846163466539,-1.42172239784));
#14762=CARTESIAN_POINT('Ctrl Pts',(2.347729791075,-1.983746799872,0.1696055881918));
#14763=CARTESIAN_POINT('Ctrl Pts',(1.885214331281,-2.075469022094,1.173320266948));
#14764=CARTESIAN_POINT('Ctrl Pts',(1.516049262601,-2.121330133205,1.537366472129));
#14765=CARTESIAN_POINT('Ctrl Pts',(-2.053521584663,2.153834933397,0.5656340822739));
#14766=CARTESIAN_POINT('Ctrl Pts',(-2.189346287892,2.107973822286,0.07252560711062));
#14767=CARTESIAN_POINT('Ctrl Pts',(-2.089406585155,2.016251600064,-1.013119392963));
#14768=CARTESIAN_POINT('Ctrl Pts',(-0.9018314834646,1.878668266731,-2.140176213964));
#14769=CARTESIAN_POINT('Ctrl Pts',(0.7340079209191,1.741084933397,-2.203251188525));
#14770=CARTESIAN_POINT('Ctrl Pts',(2.005082151636,1.603501600064,-1.171683541509));
#14771=CARTESIAN_POINT('Ctrl Pts',(2.279849870396,1.465918266731,0.4421274288044));
#14772=CARTESIAN_POINT('Ctrl Pts',(1.421766653915,1.328334933397,1.836236754172));
#14773=CARTESIAN_POINT('Ctrl Pts',(-0.1427858438013,1.190751600064,2.317930303956));
#14774=CARTESIAN_POINT('Ctrl Pts',(-1.636388843192,1.053168266731,1.647853010538));
#14775=CARTESIAN_POINT('Ctrl Pts',(-2.316876854778,0.9155849333973,0.1589644848776));
#14776=CARTESIAN_POINT('Ctrl Pts',(-1.846118234175,0.778001600064,-1.408912897352));
#14777=CARTESIAN_POINT('Ctrl Pts',(-0.4580309987508,0.6404182667307,-2.276707200713));
#14778=CARTESIAN_POINT('Ctrl Pts',(1.15764996827,0.5028349333973,-2.013214998089));
#14779=CARTESIAN_POINT('Ctrl Pts',(2.19809939426,0.365251600064,-0.7493644839955));
#14780=CARTESIAN_POINT('Ctrl Pts',(2.146322208353,0.2276682667307,0.8868421814655));
#14781=CARTESIAN_POINT('Ctrl Pts',(1.02804628286,0.09008493339734,2.082380588953));
#14782=CARTESIAN_POINT('Ctrl Pts',(-0.6010616419805,-0.047498399936,2.243192586352));
#14783=CARTESIAN_POINT('Ctrl Pts',(-1.931504491699,-0.1850817332693,1.289371348951));
#14784=CARTESIAN_POINT('Ctrl Pts',(-2.302190647873,-0.3226650666027,-0.3051332458796));
#14785=CARTESIAN_POINT('Ctrl Pts',(-1.528927673474,-0.460248399936,-1.748018376964));
#14786=CARTESIAN_POINT('Ctrl Pts',(0.004053217832441,-0.5978317332693,-2.32232031576));
#14787=CARTESIAN_POINT('Ctrl Pts',(1.535020080995,-0.7354150666027,-1.742670773421));
#14788=CARTESIAN_POINT('Ctrl Pts',(2.303241737861,-0.872998399936,-0.297095243739));
#14789=CARTESIAN_POINT('Ctrl Pts',(1.926991971239,-1.010581733269,1.296105709592));
#14790=CARTESIAN_POINT('Ctrl Pts',(0.593227803405,-1.148165066603,2.245276990425));
#14791=CARTESIAN_POINT('Ctrl Pts',(-1.035308983945,-1.285748399936,2.078779449328));
#14792=CARTESIAN_POINT('Ctrl Pts',(-2.14940441763,-1.423331733269,0.8793443495176));
#14793=CARTESIAN_POINT('Ctrl Pts',(-2.195471618979,-1.560915066603,-0.7570313501432));
#14794=CARTESIAN_POINT('Ctrl Pts',(-1.150610309237,-1.698498399936,-2.017248787961));
#14795=CARTESIAN_POINT('Ctrl Pts',(0.4659560881674,-1.836081733269,-2.27507546064));
#14796=CARTESIAN_POINT('Ctrl Pts',(1.851097081595,-1.973665066603,-1.402531228136));
#14797=CARTESIAN_POINT('Ctrl Pts',(2.316038878061,-2.111248399936,0.1673161612047));
#14798=CARTESIAN_POINT('Ctrl Pts',(1.85976669944,-2.202970622158,1.157482162128));
#14799=CARTESIAN_POINT('Ctrl Pts',(1.495584818401,-2.248831733269,1.516614276827));
#14800=CARTESIAN_POINT('Ctrl Pts',(-2.157170361559,1.938833333333,0.5941837119619));
#14801=CARTESIAN_POINT('Ctrl Pts',(-2.299850636439,1.892972222222,0.07618624088569));
#14802=CARTESIAN_POINT('Ctrl Pts',(-2.19486660983,1.80125,-1.064255249881));
#14803=CARTESIAN_POINT('Ctrl Pts',(-0.9473502308328,1.663666666667,-2.24819876828));
#14804=CARTESIAN_POINT('Ctrl Pts',(0.7710559966752,1.526083333333,-2.31445736848));
#14805=CARTESIAN_POINT('Ctrl Pts',(2.10628601243,1.3885,-1.230822713405));
#14806=CARTESIAN_POINT('Ctrl Pts',(2.394922267169,1.250916666667,0.4644432240559));
#14807=CARTESIAN_POINT('Ctrl Pts',(1.493528439041,1.113333333333,1.928918367593));
#14808=CARTESIAN_POINT('Ctrl Pts',(-0.1499927697857,0.97575,2.434924760079));
#14809=CARTESIAN_POINT('Ctrl Pts',(-1.718983398511,0.8381666666667,1.73102620449));
#14810=CARTESIAN_POINT('Ctrl Pts',(-2.433818139452,0.7005833333333,0.1669880063007));
#14811=CARTESIAN_POINT('Ctrl Pts',(-1.939298602186,0.563,-1.480025906173));
#14812=CARTESIAN_POINT('Ctrl Pts',(-0.4811495055907,0.4254166666667,-2.391620975404));
#14813=CARTESIAN_POINT('Ctrl Pts',(1.216080814179,0.2878333333333,-2.114829353515));
#14814=CARTESIAN_POINT('Ctrl Pts',(2.309045544236,0.15025,-0.7871876618941));
#14815=CARTESIAN_POINT('Ctrl Pts',(2.25465497358,0.01266666666667,0.9316043637066));
#14816=CARTESIAN_POINT('Ctrl Pts',(1.079935554736,-0.1249166666667,2.187485985794));
#14817=CARTESIAN_POINT('Ctrl Pts',(-0.6313994307312,-0.2625,2.356414755359));
#14818=CARTESIAN_POINT('Ctrl Pts',(-2.028994617748,-0.4000833333333,1.354450656752));
#14819=CARTESIAN_POINT('Ctrl Pts',(-2.418390665742,-0.5376666666667,-0.3205344415436));
#14820=CARTESIAN_POINT('Ctrl Pts',(-1.606098268856,-0.67525,-1.836247284864));
#14821=CARTESIAN_POINT('Ctrl Pts',(0.004257798623803,-0.8128333333333,-2.439536351903));
#14822=CARTESIAN_POINT('Ctrl Pts',(1.612498182562,-0.9504166666667,-1.830629768129));
#14823=CARTESIAN_POINT('Ctrl Pts',(2.419494808103,-1.088,-0.3120907319116));
#14824=CARTESIAN_POINT('Ctrl Pts',(2.024254333806,-1.225583333333,1.36152492531));
#14825=CARTESIAN_POINT('Ctrl Pts',(0.6231701895493,-1.363166666667,2.358604366961));
#14826=CARTESIAN_POINT('Ctrl Pts',(-1.087564831021,-1.50075,2.183703083425));
#14827=CARTESIAN_POINT('Ctrl Pts',(-2.25789275328,-1.638333333333,0.9237280886409));
#14828=CARTESIAN_POINT('Ctrl Pts',(-2.306285135485,-1.775916666667,-0.7952415029365));
#14829=CARTESIAN_POINT('Ctrl Pts',(-1.208685837698,-1.9135,-2.119066743579));
#14830=CARTESIAN_POINT('Ctrl Pts',(0.4894746033787,-2.051083333333,-2.389906875417));
#14831=CARTESIAN_POINT('Ctrl Pts',(1.944528750322,-2.188666666667,-1.473322130671));
#14832=CARTESIAN_POINT('Ctrl Pts',(2.432937866972,-2.32625,0.1757612224075));
#14833=CARTESIAN_POINT('Ctrl Pts',(1.953635955623,-2.417972222222,1.215904538245));
#14834=CARTESIAN_POINT('Ctrl Pts',(1.57107247742,-2.463833333333,1.593163369853));
#14835=CARTESIAN_POINT('Ctrl Pts',(-2.37767976724,1.824458133325,0.6549221216513));
#14836=CARTESIAN_POINT('Ctrl Pts',(-2.534945048097,1.778597022214,0.08397412032173));
#14837=CARTESIAN_POINT('Ctrl Pts',(-2.419229386322,1.686874799992,-1.173045124258));
#14838=CARTESIAN_POINT('Ctrl Pts',(-1.044189887123,1.549291466659,-2.478013243336));
#14839=CARTESIAN_POINT('Ctrl Pts',(0.8498745742914,1.411708133325,-2.551044903657));
#14840=CARTESIAN_POINT('Ctrl Pts',(2.321593938533,1.274124799992,-1.3566393804));
#14841=CARTESIAN_POINT('Ctrl Pts',(2.639735053028,1.136541466659,0.5119193534958));
#14842=CARTESIAN_POINT('Ctrl Pts',(1.646199305622,0.9989581333253,2.126095489263));
#14843=CARTESIAN_POINT('Ctrl Pts',(-0.1653252706912,0.861374799992,2.683826664765));
#14844=CARTESIAN_POINT('Ctrl Pts',(-1.894700631761,0.7237914666587,1.907974472635));
#14845=CARTESIAN_POINT('Ctrl Pts',(-2.682606923607,0.5862081333253,0.184057787474));
#14846=CARTESIAN_POINT('Ctrl Pts',(-2.137536808044,0.448624799992,-1.63131652224));
#14847=CARTESIAN_POINT('Ctrl Pts',(-0.530333377858,0.3110414666587,-2.636096297938));
#14848=CARTESIAN_POINT('Ctrl Pts',(1.340390540649,0.1734581333253,-2.331010593612));
#14849=CARTESIAN_POINT('Ctrl Pts',(2.54507987408,0.035874799992,-0.8676552441385));
#14850=CARTESIAN_POINT('Ctrl Pts',(2.485129412271,-0.1017085333413,1.026834452267));
#14851=CARTESIAN_POINT('Ctrl Pts',(1.190328294963,-0.2392918666747,2.411094303088));
#14852=CARTESIAN_POINT('Ctrl Pts',(-0.6959420907358,-0.376875200008,2.597291241752));
#14853=CARTESIAN_POINT('Ctrl Pts',(-2.236401693825,-0.5144585333413,1.492904769912));
#14854=CARTESIAN_POINT('Ctrl Pts',(-2.665602428852,-0.6520418666747,-0.3532999849911));
#14855=CARTESIAN_POINT('Ctrl Pts',(-1.770276203545,-0.789625200008,-2.023951420191));
#14856=CARTESIAN_POINT('Ctrl Pts',(0.004693037611301,-0.9272085333413,-2.688909660883));
#14857=CARTESIAN_POINT('Ctrl Pts',(1.777330326669,-1.064791866675,-2.017759671907));
#14858=CARTESIAN_POINT('Ctrl Pts',(2.666819438411,-1.202375200008,-0.3439931458512));
#14859=CARTESIAN_POINT('Ctrl Pts',(2.231176850475,-1.339958533341,1.50070218152));
#14860=CARTESIAN_POINT('Ctrl Pts',(0.6868716433541,-1.477541866675,2.599704678955));
#14861=CARTESIAN_POINT('Ctrl Pts',(-1.198737448077,-1.615125200008,2.406924706386));
#14862=CARTESIAN_POINT('Ctrl Pts',(-2.488698162992,-1.752708533341,1.018153051763));
#14863=CARTESIAN_POINT('Ctrl Pts',(-2.542037291931,-1.890291866675,-0.8765323616979));
#14864=CARTESIAN_POINT('Ctrl Pts',(-1.332239637841,-2.027875200008,-2.335681136467));
#14865=CARTESIAN_POINT('Ctrl Pts',(0.5395094804615,-2.165458533341,-2.634206979907));
#14866=CARTESIAN_POINT('Ctrl Pts',(2.143301590291,-2.303041866675,-1.623927476082));
#14867=CARTESIAN_POINT('Ctrl Pts',(2.681636668265,-2.440625200008,0.1937278157678));
#14868=CARTESIAN_POINT('Ctrl Pts',(2.153339748689,-2.53234742223,1.340196245508));
#14869=CARTESIAN_POINT('Ctrl Pts',(1.731670019669,-2.578208533341,1.756019078471));
#14870=CARTESIAN_POINT('Ctrl Pts',(-2.565745420624,1.884351681926,0.7067240330865));
#14871=CARTESIAN_POINT('Ctrl Pts',(-2.735449802072,1.838490570815,0.09061616187131));
#14872=CARTESIAN_POINT('Ctrl Pts',(-2.610581460513,1.746768348593,-1.26582864405));
#14873=CARTESIAN_POINT('Ctrl Pts',(-1.12678143544,1.60918501526,-2.674014902652));
#14874=CARTESIAN_POINT('Ctrl Pts',(0.9170965018656,1.471601681926,-2.75282309651));
#14875=CARTESIAN_POINT('Ctrl Pts',(2.505223410826,1.334018348593,-1.463944525103));
#14876=CARTESIAN_POINT('Ctrl Pts',(2.848528307842,1.19643501526,0.5524102762102));
#14877=CARTESIAN_POINT('Ctrl Pts',(1.77640756675,1.058851681926,2.294261759109));
#14878=CARTESIAN_POINT('Ctrl Pts',(-0.1784018865929,0.9212683485929,2.89610740258));
#14879=CARTESIAN_POINT('Ctrl Pts',(-2.044564426368,0.7836850152596,2.058888178837));
#14880=CARTESIAN_POINT('Ctrl Pts',(-2.894791184419,0.6461016819263,0.1986160759949));
#14881=CARTESIAN_POINT('Ctrl Pts',(-2.306608043782,0.5085183485929,-1.760347610387));
#14882=CARTESIAN_POINT('Ctrl Pts',(-0.5722807816221,0.3709350152596,-2.844601740716));
#14883=CARTESIAN_POINT('Ctrl Pts',(1.446410462377,0.2333516819263,-2.515384888406));
#14884=CARTESIAN_POINT('Ctrl Pts',(2.746386255211,0.09576834859292,-0.9362835567687));
#14885=CARTESIAN_POINT('Ctrl Pts',(2.681693934163,-0.04181498474041,1.108053250039));
#14886=CARTESIAN_POINT('Ctrl Pts',(1.284478849473,-0.1793983180737,2.601802922359));
#14887=CARTESIAN_POINT('Ctrl Pts',(-0.7509885296274,-0.3169816514071,2.802727348471));
#14888=CARTESIAN_POINT('Ctrl Pts',(-2.413292775447,-0.4545649847404,1.610988001667));
#14889=CARTESIAN_POINT('Ctrl Pts',(-2.87644169718,-0.5921483180737,-0.3812447038019));
#14890=CARTESIAN_POINT('Ctrl Pts',(-1.910298487233,-0.7297316514071,-2.184038472913));
#14891=CARTESIAN_POINT('Ctrl Pts',(0.005064239485027,-0.8673149847404,-2.901592444844));
#14892=CARTESIAN_POINT('Ctrl Pts',(1.91791056534,-1.004898318074,-2.177356980299));
#14893=CARTESIAN_POINT('Ctrl Pts',(2.877754967682,-1.142481651407,-0.3712017281949));
#14894=CARTESIAN_POINT('Ctrl Pts',(2.407654666361,-1.28006498474,1.619402159621));
#14895=CARTESIAN_POINT('Ctrl Pts',(0.7412006434902,-1.417648318074,2.805331679608));
#14896=CARTESIAN_POINT('Ctrl Pts',(-1.293553135418,-1.555231651407,2.597303526019));
#14897=CARTESIAN_POINT('Ctrl Pts',(-2.685544959835,-1.69281498474,1.098685182945));
#14898=CARTESIAN_POINT('Ctrl Pts',(-2.743103016096,-1.830398318074,-0.9458628214115));
#14899=CARTESIAN_POINT('Ctrl Pts',(-1.43761485338,-1.967981651407,-2.520424853883));
#14900=CARTESIAN_POINT('Ctrl Pts',(0.5821826799174,-2.10556498474,-2.842562984635));
#14901=CARTESIAN_POINT('Ctrl Pts',(2.31282879893,-2.243148318074,-1.752374118075));
#14902=CARTESIAN_POINT('Ctrl Pts',(2.893744185478,-2.380731651407,0.2090509676711));
#14903=CARTESIAN_POINT('Ctrl Pts',(2.323660938436,-2.472453873629,1.44620079921));
#14904=CARTESIAN_POINT('Ctrl Pts',(1.868638697361,-2.51831498474,1.89491367643));
#14905=CARTESIAN_POINT('Ctrl Pts',(-2.691657648987,2.002509974399,0.7414060389974));
#14906=CARTESIAN_POINT('Ctrl Pts',(-2.869690158652,1.956648863288,0.09506308898078));
#14907=CARTESIAN_POINT('Ctrl Pts',(-2.738693987334,1.864926641066,-1.32794833216));
#14908=CARTESIAN_POINT('Ctrl Pts',(-1.182077475443,1.727343307732,-2.805240382922));
#14909=CARTESIAN_POINT('Ctrl Pts',(0.9621023949859,1.589759974399,-2.887916035812));
#14910=CARTESIAN_POINT('Ctrl Pts',(2.628165562323,1.452176641066,-1.535786616635));
#14911=CARTESIAN_POINT('Ctrl Pts',(2.988317915928,1.314593307732,0.5795194384402));
#14912=CARTESIAN_POINT('Ctrl Pts',(1.863583571592,1.177009974399,2.406851109641));
#14913=CARTESIAN_POINT('Ctrl Pts',(-0.1871568390151,1.039426641066,3.038231922694));
#14914=CARTESIAN_POINT('Ctrl Pts',(-2.144900048479,0.9018433077322,2.159926729453));
#14915=CARTESIAN_POINT('Ctrl Pts',(-3.036851112013,0.7642599743989,0.2083630261468));
#14916=CARTESIAN_POINT('Ctrl Pts',(-2.419803279919,0.6266766410655,-1.846735483687));
#14917=CARTESIAN_POINT('Ctrl Pts',(-0.6003650755214,0.4890933077322,-2.984198655165));
#14918=CARTESIAN_POINT('Ctrl Pts',(1.517392081591,0.3515099743989,-2.638825707572));
#14919=CARTESIAN_POINT('Ctrl Pts',(2.881163310862,0.2139266410655,-0.9822310416849));
#14920=CARTESIAN_POINT('Ctrl Pts',(2.813296257732,0.07634330773221,1.162430216957));
#14921=CARTESIAN_POINT('Ctrl Pts',(1.347513783853,-0.06124002560112,2.729484648334));
#14922=CARTESIAN_POINT('Ctrl Pts',(-0.7878427858918,-0.1988233589345,2.940269305325));
#14923=CARTESIAN_POINT('Ctrl Pts',(-2.531723492933,-0.3364066922678,1.69004615277));
#14924=CARTESIAN_POINT('Ctrl Pts',(-3.017601136046,-0.4739900256011,-0.3999540308542));
#14925=CARTESIAN_POINT('Ctrl Pts',(-2.004045098816,-0.6115733589345,-2.291218689916));
#14926=CARTESIAN_POINT('Ctrl Pts',(0.005312763626742,-0.7491566922678,-3.043986139712));
#14927=CARTESIAN_POINT('Ctrl Pts',(2.012030734529,-0.8867400256011,-2.284209307552));
#14928=CARTESIAN_POINT('Ctrl Pts',(3.018978854414,-1.024323358934,-0.3894182029838));
#14929=CARTESIAN_POINT('Ctrl Pts',(2.525808697441,-1.161906692268,1.698873229859));
#14930=CARTESIAN_POINT('Ctrl Pts',(0.777574565835,-1.299490025601,2.943001442258));
#14931=CARTESIAN_POINT('Ctrl Pts',(-1.357033384268,-1.437073358934,2.724764447149));
#14932=CARTESIAN_POINT('Ctrl Pts',(-2.817336269894,-1.574656692268,1.15260241828));
#14933=CARTESIAN_POINT('Ctrl Pts',(-2.877718948998,-1.712240025601,-0.992280402288));
#14934=CARTESIAN_POINT('Ctrl Pts',(-1.508164834006,-1.849823358934,-2.64411300596));
#14935=CARTESIAN_POINT('Ctrl Pts',(0.6107529028062,-1.987406692268,-2.982059848502));
#14936=CARTESIAN_POINT('Ctrl Pts',(2.426329314435,-2.124990025601,-1.838370697611));
#14937=CARTESIAN_POINT('Ctrl Pts',(3.035752732303,-2.262573358934,0.2193100031036));
#14938=CARTESIAN_POINT('Ctrl Pts',(2.437693033892,-2.354295581157,1.517172129345));
#14939=CARTESIAN_POINT('Ctrl Pts',(1.960340882815,-2.400156692268,1.987905288785));
#14940=CARTESIAN_POINT('Ctrl Pts',(-2.759938298802,2.158874760259,0.7602136634136));
#14941=CARTESIAN_POINT('Ctrl Pts',(-2.942487049769,2.113013649148,0.0974746027524));
#14942=CARTESIAN_POINT('Ctrl Pts',(-2.808167831889,2.021291426926,-1.361635073516));
#14943=CARTESIAN_POINT('Ctrl Pts',(-1.212063836518,1.883708093593,-2.876402343769));
#14944=CARTESIAN_POINT('Ctrl Pts',(0.9865085362136,1.746124760259,-2.961175272033));
#14945=CARTESIAN_POINT('Ctrl Pts',(2.694835576054,1.608541426926,-1.574745697557));
#14946=CARTESIAN_POINT('Ctrl Pts',(3.064124097754,1.470958093593,0.594220403049));
#14947=CARTESIAN_POINT('Ctrl Pts',(1.91085804474,1.333374760259,2.467906926987));
#14948=CARTESIAN_POINT('Ctrl Pts',(-0.1919045418257,1.195791426926,3.115304298539));
#14949=CARTESIAN_POINT('Ctrl Pts',(-2.199310819906,1.058208093593,2.214718690345));
#14950=CARTESIAN_POINT('Ctrl Pts',(-3.11388846013,0.9206247602593,0.2136486771017));
#14951=CARTESIAN_POINT('Ctrl Pts',(-2.481187661562,0.7830414269259,-1.893582562813));
#14952=CARTESIAN_POINT('Ctrl Pts',(-0.6155948420179,0.6454580935926,-3.059900341606));
#14953=CARTESIAN_POINT('Ctrl Pts',(1.555884538978,0.5078747602593,-2.705766142633));
#14954=CARTESIAN_POINT('Ctrl Pts',(2.954251247272,0.3702914269259,-1.00714779654));
#14955=CARTESIAN_POINT('Ctrl Pts',(2.884662576057,0.2327080935926,1.191918176025));
#14956=CARTESIAN_POINT('Ctrl Pts',(1.381696851982,0.09512476025927,2.798724874897));
#14957=CARTESIAN_POINT('Ctrl Pts',(-0.8078283949059,-0.04245857307406,3.014856613586));
#14958=CARTESIAN_POINT('Ctrl Pts',(-2.595947011594,-0.1800419064074,1.732918413874));
#14959=CARTESIAN_POINT('Ctrl Pts',(-3.094150160224,-0.3176252397407,-0.4100998683581));
#14960=CARTESIAN_POINT('Ctrl Pts',(-2.05488273103,-0.4552085730741,-2.349341200806));
#14961=CARTESIAN_POINT('Ctrl Pts',(0.00544753520622,-0.5927919064074,-3.121204485709));
#14962=CARTESIAN_POINT('Ctrl Pts',(2.063070942429,-0.7303752397407,-2.342154007871));
#14963=CARTESIAN_POINT('Ctrl Pts',(3.095562827875,-0.8679585730741,-0.3992967727786));
#14964=CARTESIAN_POINT('Ctrl Pts',(2.589882172473,-1.005541906407,1.74196941192));
#14965=CARTESIAN_POINT('Ctrl Pts',(0.7972996956837,-1.143125239741,3.017658058028));
#14966=CARTESIAN_POINT('Ctrl Pts',(-1.391457940947,-1.280708573074,2.793884933966));
#14967=CARTESIAN_POINT('Ctrl Pts',(-2.888805073264,-1.418291906407,1.181841070576));
#14968=CARTESIAN_POINT('Ctrl Pts',(-2.950719510528,-1.555875239741,-1.01745208439));
#14969=CARTESIAN_POINT('Ctrl Pts',(-1.546423219107,-1.693458573074,-2.711187566611));
#14970=CARTESIAN_POINT('Ctrl Pts',(0.6262461826055,-1.831041906407,-3.057707278746));
#14971=CARTESIAN_POINT('Ctrl Pts',(2.487879245318,-1.968625239741,-1.88500558295));
#14972=CARTESIAN_POINT('Ctrl Pts',(3.112762217264,-2.106208573074,0.2248733515957));
#14973=CARTESIAN_POINT('Ctrl Pts',(2.499531234031,-2.197930795296,1.555659007092));
#14974=CARTESIAN_POINT('Ctrl Pts',(2.010069847933,-2.243791906407,2.038333494221));
#14975=CARTESIAN_POINT('Ctrl Pts',(-2.744223782437,2.268306095628,0.755885164454));
#14976=CARTESIAN_POINT('Ctrl Pts',(-2.925733138669,2.222444984517,0.09691960257691));
#14977=CARTESIAN_POINT('Ctrl Pts',(-2.792178706563,2.130722762294,-1.353882205759));
#14978=CARTESIAN_POINT('Ctrl Pts',(-1.20516259637,1.993139428961,-2.860024705282));
#14979=CARTESIAN_POINT('Ctrl Pts',(0.9808915611733,1.855556095628,-2.944314954071));
#14980=CARTESIAN_POINT('Ctrl Pts',(2.679491741092,1.717972762294,-1.565779422098));
#14981=CARTESIAN_POINT('Ctrl Pts',(3.046677610526,1.580389428961,0.5908370352931));
#14982=CARTESIAN_POINT('Ctrl Pts',(1.899978015274,1.442806095628,2.453855176696));
#14983=CARTESIAN_POINT('Ctrl Pts',(-0.1908118771584,1.305222762294,3.09756640186));
#14984=CARTESIAN_POINT('Ctrl Pts',(-2.186788400152,1.167639428961,2.202108541372));
#14985=CARTESIAN_POINT('Ctrl Pts',(-3.096158624942,1.030056095628,0.212432205837));
#14986=CARTESIAN_POINT('Ctrl Pts',(-2.467060293522,0.8924727622944,-1.882800896359));
#14987=CARTESIAN_POINT('Ctrl Pts',(-0.6120897726388,0.754889428961,-3.04247790357));
#14988=CARTESIAN_POINT('Ctrl Pts',(1.547025655045,0.6173060956277,-2.690360071292));
#14989=CARTESIAN_POINT('Ctrl Pts',(2.937430353272,0.4797227622944,-1.001413305832));
#14990=CARTESIAN_POINT('Ctrl Pts',(2.86823790552,0.342139428961,1.18513164109));
#14991=CARTESIAN_POINT('Ctrl Pts',(1.373829756619,0.2045560956277,2.78278951581));
#14992=CARTESIAN_POINT('Ctrl Pts',(-0.8032287875387,0.06697276229438,2.997690645196));
#14993=CARTESIAN_POINT('Ctrl Pts',(-2.581166227612,-0.07061057103895,1.723051535767));
#14994=CARTESIAN_POINT('Ctrl Pts',(-3.076532710823,-0.2081939043723,-0.407764844747));
#14995=CARTESIAN_POINT('Ctrl Pts',(-2.043182654865,-0.3457772377056,-2.335964539174));
#14996=CARTESIAN_POINT('Ctrl Pts',(0.005416518070365,-0.483360571039,-3.103432994589));
#14997=CARTESIAN_POINT('Ctrl Pts',(2.051324244287,-0.6209439043723,-2.328818268625));
#14998=CARTESIAN_POINT('Ctrl Pts',(3.077937335037,-0.7585272377056,-0.3970232597536));
#14999=CARTESIAN_POINT('Ctrl Pts',(2.575135920428,-0.896110571039,1.732050999308));
#15000=CARTESIAN_POINT('Ctrl Pts',(0.7927600365466,-1.033693904372,3.000476138795));
#15001=CARTESIAN_POINT('Ctrl Pts',(-1.383535267967,-1.171277237706,2.777977132499));
#15002=CARTESIAN_POINT('Ctrl Pts',(-2.872356816207,-1.308860571039,1.17511191259));
#15003=CARTESIAN_POINT('Ctrl Pts',(-2.933918725503,-1.446443904372,-1.011658923203));
#15004=CARTESIAN_POINT('Ctrl Pts',(-1.537618205967,-1.584027237706,-2.695750626806));
#15005=CARTESIAN_POINT('Ctrl Pts',(0.6226804667018,-1.721610571039,-3.040297327555));
#15006=CARTESIAN_POINT('Ctrl Pts',(2.473713776788,-1.859193904372,-1.87427275204));
#15007=CARTESIAN_POINT('Ctrl Pts',(3.095038794669,-1.996777237706,0.2235929693621));
#15008=CARTESIAN_POINT('Ctrl Pts',(2.485299421493,-2.088499459928,1.546801407291));
#15009=CARTESIAN_POINT('Ctrl Pts',(1.998624927033,-2.134360571039,2.026727645979));
#15010=CARTESIAN_POINT('Ctrl Pts',(-2.723241031212,2.319248086811,0.7501055518504));
#15011=CARTESIAN_POINT('Ctrl Pts',(-2.90336253938,2.2733869757,0.09617854059695));
#15012=CARTESIAN_POINT('Ctrl Pts',(-2.770829284715,2.181664753478,-1.343530217087));
#15013=CARTESIAN_POINT('Ctrl Pts',(-1.195947740385,2.044081420145,-2.838156522639));
#15014=CARTESIAN_POINT('Ctrl Pts',(0.9733915155363,1.906498086811,-2.921802275403));
#15015=CARTESIAN_POINT('Ctrl Pts',(2.659003940873,1.768914753478,-1.553807235173));
#15016=CARTESIAN_POINT('Ctrl Pts',(3.023382251462,1.631331420145,0.586319405716));
#15017=CARTESIAN_POINT('Ctrl Pts',(1.885450495222,1.493748086811,2.435092627868));
#15018=CARTESIAN_POINT('Ctrl Pts',(-0.1893529006074,1.356164753478,3.07388193938));
#15019=CARTESIAN_POINT('Ctrl Pts',(-2.1700678844,1.218581420145,2.185270885497));
#15020=CARTESIAN_POINT('Ctrl Pts',(-3.072484926538,1.080998086811,0.2108079169741));
#15021=CARTESIAN_POINT('Ctrl Pts',(-2.448196776368,0.9434147534781,-1.868404715163));
#15022=CARTESIAN_POINT('Ctrl Pts',(-0.6074096414087,0.8058314201447,-3.019214656103));
#15023=CARTESIAN_POINT('Ctrl Pts',(1.535196862268,0.6682480868114,-2.669789170172));
#15024=CARTESIAN_POINT('Ctrl Pts',(2.914970315305,0.5306647534781,-0.9937563478226));
#15025=CARTESIAN_POINT('Ctrl Pts',(2.846306923502,0.3930814201447,1.176069944827));
#15026=CARTESIAN_POINT('Ctrl Pts',(1.363325245947,0.2554980868114,2.761511885139));
#15027=CARTESIAN_POINT('Ctrl Pts',(-0.797087178413,0.1179147534781,2.974769847899));
#15028=CARTESIAN_POINT('Ctrl Pts',(-2.561430239181,-0.01966857985526,1.70987682241));
#15029=CARTESIAN_POINT('Ctrl Pts',(-3.053009075134,-0.1572519131886,-0.4046470129032));
#15030=CARTESIAN_POINT('Ctrl Pts',(-2.02756017042,-0.2948352465219,-2.318103400039));
#15031=CARTESIAN_POINT('Ctrl Pts',(0.005375102551739,-0.4324185798553,-3.079703675251));
#15032=CARTESIAN_POINT('Ctrl Pts',(2.035639508015,-0.5700019131886,-2.311011770959));
#15033=CARTESIAN_POINT('Ctrl Pts',(3.054402959379,-0.7075852465219,-0.3939875596977));
#15034=CARTESIAN_POINT('Ctrl Pts',(2.55544604064,-0.8451685798553,1.718807474687));
#15035=CARTESIAN_POINT('Ctrl Pts',(0.7866984730786,-0.9827519131886,2.977534043191));
#15036=CARTESIAN_POINT('Ctrl Pts',(-1.372956547484,-1.120335246522,2.756736298041));
#15037=CARTESIAN_POINT('Ctrl Pts',(-2.850394340374,-1.257918579855,1.166126828691));
#15038=CARTESIAN_POINT('Ctrl Pts',(-2.911485537975,-1.395501913189,-1.003923625649));
#15039=CARTESIAN_POINT('Ctrl Pts',(-1.525861343972,-1.533085246522,-2.67513850868));
#15040=CARTESIAN_POINT('Ctrl Pts',(0.6179193574188,-1.670668579855,-3.017050753102));
#15041=CARTESIAN_POINT('Ctrl Pts',(2.454799386092,-1.808251913189,-1.859941778329));
#15042=CARTESIAN_POINT('Ctrl Pts',(3.071373658657,-1.945835246522,0.2218833436086));
#15043=CARTESIAN_POINT('Ctrl Pts',(2.466296445201,-2.037557468744,1.534974329146));
#15044=CARTESIAN_POINT('Ctrl Pts',(1.983343137733,-2.083418579855,2.011230979028));
#15045=CARTESIAN_POINT('Ctrl Pts',(2.01902946445913,-2.11666666786796,0.734863845645197));
#15046=CARTESIAN_POINT('Ctrl Pts',(2.01902946451889,-2.11668202258293,0.734863837959268));
#15047=CARTESIAN_POINT('Ctrl Pts',(2.01902946584361,-2.1166973773117,0.734863830734622));
#15048=CARTESIAN_POINT('Ctrl Pts',(2.0190294684334,-2.11671273205414,0.734863823971304));
#15049=CARTESIAN_POINT('Ctrl Pts',(2.01903548208762,-2.15236732805478,0.734848119158269));
#15050=CARTESIAN_POINT('Ctrl Pts',(2.02586252056251,-2.18809959722609,0.737319747367766));
#15051=CARTESIAN_POINT('Ctrl Pts',(2.03820710077089,-2.22243716863227,0.741802872331295));
#15052=CARTESIAN_POINT('Ctrl Pts',(2.04907580053001,-2.25266944447893,0.745750008514841));
#15053=CARTESIAN_POINT('Ctrl Pts',(2.06422244902162,-2.28182080703269,0.75125674949461));
#15054=CARTESIAN_POINT('Ctrl Pts',(2.08275044399805,-2.3088469914139,0.757996028301507));
#15055=CARTESIAN_POINT('Ctrl Pts',(2.09424913019561,-2.32561975142987,0.762178502028261));
#15056=CARTESIAN_POINT('Ctrl Pts',(2.1070499859288,-2.34157319175473,0.766835634157785));
#15057=CARTESIAN_POINT('Ctrl Pts',(2.12093514751278,-2.35644804570745,0.771887967645838));
#15058=CARTESIAN_POINT('Ctrl Pts',(2.12121072935012,-2.35674327018558,0.771988242413044));
#15059=CARTESIAN_POINT('Ctrl Pts',(2.12148674218689,-2.35703807399843,0.77208867472817));
#15060=CARTESIAN_POINT('Ctrl Pts',(2.12176318420811,-2.35733245490323,0.772189263929199));
#15061=CARTESIAN_POINT('Ctrl Pts',(2.14134918971209,-2.37818943603857,0.779316040952179));
#15062=CARTESIAN_POINT('Ctrl Pts',(2.16309415443761,-2.3969226989842,0.787232005697749));
#15063=CARTESIAN_POINT('Ctrl Pts',(2.18632484782624,-2.41273811410247,0.795691621595359));
#15064=CARTESIAN_POINT('Ctrl Pts',(2.21101485867412,-2.42954702997516,0.804682657927619));
#15065=CARTESIAN_POINT('Ctrl Pts',(2.23738150094186,-2.44305736749398,0.814287210804268));
#15066=CARTESIAN_POINT('Ctrl Pts',(2.2645681620712,-2.45234913529765,0.82419282825343));
#15067=CARTESIAN_POINT('Ctrl Pts',(2.28827459351538,-2.46045144162298,0.832830403859112));
#15068=CARTESIAN_POINT('Ctrl Pts',(2.31260281779126,-2.4653456070908,0.841696272796586));
#15069=CARTESIAN_POINT('Ctrl Pts',(2.33697436671365,-2.46646509645855,0.850579343032716));
#15070=CARTESIAN_POINT('Ctrl Pts',(2.34055223916708,-2.46662944342654,0.851883424788085));
#15071=CARTESIAN_POINT('Ctrl Pts',(2.34413104789601,-2.46671253148602,0.8531878779859));
#15072=CARTESIAN_POINT('Ctrl Pts',(2.34770897025998,-2.46671266849111,0.854492037291276));
#15073=CARTESIAN_POINT('Ctrl Pts',(2.3482169537651,-2.46671268794271,0.854677198216468));
#15074=CARTESIAN_POINT('Ctrl Pts',(2.34872491941112,-2.46671103535315,0.85486235322026));
#15075=CARTESIAN_POINT('Ctrl Pts',(2.34923286192811,-2.46670771626141,0.8550475003789));
#15076=CARTESIAN_POINT('Ctrl Pts',(2.3791440767032,-2.46651226488167,0.865950262486324));
#15077=CARTESIAN_POINT('Ctrl Pts',(2.40903830687,-2.4605323337516,0.876843657964342));
#15078=CARTESIAN_POINT('Ctrl Pts',(2.43787213578489,-2.44985748919329,0.887348258852877));
#15079=CARTESIAN_POINT('Ctrl Pts',(2.45728477633215,-2.44267055190099,0.894420578028505));
#15080=CARTESIAN_POINT('Ctrl Pts',(2.47621682134733,-2.43335694704768,0.901316688346371));
#15081=CARTESIAN_POINT('Ctrl Pts',(2.49435736808247,-2.42225965114417,0.907923562114362));
#15082=CARTESIAN_POINT('Ctrl Pts',(2.51927659281981,-2.40701556756533,0.916999262788638));
#15083=CARTESIAN_POINT('Ctrl Pts',(2.5426999565375,-2.38840626533803,0.925528330549401));
#15084=CARTESIAN_POINT('Ctrl Pts',(2.56389875562379,-2.36732903978015,0.933245972984017));
#15085=CARTESIAN_POINT('Ctrl Pts',(2.56800440129363,-2.36324693968138,0.934740675826101));
#15086=CARTESIAN_POINT('Ctrl Pts',(2.57202675117484,-2.35907226476846,0.936204996181314));
#15087=CARTESIAN_POINT('Ctrl Pts',(2.57596073679862,-2.35481151043351,0.937637092926701));
#15088=CARTESIAN_POINT('Ctrl Pts',(2.58917727405375,-2.34049716773172,0.942448335721781));
#15089=CARTESIAN_POINT('Ctrl Pts',(2.60140094411319,-2.32520667963406,0.946896870192865));
#15090=CARTESIAN_POINT('Ctrl Pts',(2.61244940192908,-2.30917261084363,0.950916358239321));
#15091=CARTESIAN_POINT('Ctrl Pts',(2.62939488883081,-2.28458048158927,0.957081217007656));
#15092=CARTESIAN_POINT('Ctrl Pts',(2.64357382956465,-2.25824081065372,0.962236059039643));
#15093=CARTESIAN_POINT('Ctrl Pts',(2.65420089843072,-2.23096428845327,0.966095278883079));
#15094=CARTESIAN_POINT('Ctrl Pts',(2.66348159972914,-2.207143490998,0.969465565371594));
#15095=CARTESIAN_POINT('Ctrl Pts',(2.67005398496024,-2.18260765891923,0.971847936252335));
#15096=CARTESIAN_POINT('Ctrl Pts',(2.67341809597679,-2.15787551631565,0.973060682827448));
#15097=CARTESIAN_POINT('Ctrl Pts',(2.67528171007863,-2.14417466949522,0.973732507154356));
#15098=CARTESIAN_POINT('Ctrl Pts',(2.67616137518176,-2.13041322894896,0.974045620035525));
#15099=CARTESIAN_POINT('Ctrl Pts',(2.67610312119081,-2.11667678879524,0.974016832256147));
#15100=CARTESIAN_POINT('Ctrl Pts',(2.16568648002,-1.914085246522,-0.2047176459706));
#15101=CARTESIAN_POINT('Ctrl Pts',(2.214844963183,-1.959946357633,0.3153247854411));
#15102=CARTESIAN_POINT('Ctrl Pts',(1.921795013418,-2.051668579855,1.389512218641));
#15103=CARTESIAN_POINT('Ctrl Pts',(0.5274877970284,-2.189251913189,2.312464102902));
#15104=CARTESIAN_POINT('Ctrl Pts',(-1.128979488109,-2.326835246522,2.085795659563));
#15105=CARTESIAN_POINT('Ctrl Pts',(-2.224447131318,-2.464418579855,0.8228556269872));
#15106=CARTESIAN_POINT('Ctrl Pts',(-2.214599923529,-2.602001913189,-0.8489986687962));
#15107=CARTESIAN_POINT('Ctrl Pts',(-1.104326028381,-2.739585246522,-2.09897809787));
#15108=CARTESIAN_POINT('Ctrl Pts',(0.5546826841579,-2.877168579855,-2.305986801935));
#15109=CARTESIAN_POINT('Ctrl Pts',(1.938071910246,-3.014751913189,-1.367159299658));
#15110=CARTESIAN_POINT('Ctrl Pts',(2.358441099535,-3.152335246522,0.2510038654405));
#15111=CARTESIAN_POINT('Ctrl Pts',(1.606910543807,-3.289918579855,1.744444291083));
#15112=CARTESIAN_POINT('Ctrl Pts',(0.05691270016944,-3.427501913189,2.371077457865));
#15113=CARTESIAN_POINT('Ctrl Pts',(-1.521364831366,-3.565085246522,1.819531923506));
#15114=CARTESIAN_POINT('Ctrl Pts',(-2.343682391654,-3.702668579855,0.3638684063681));
#15115=CARTESIAN_POINT('Ctrl Pts',(-2.001433743259,-3.840251913189,-1.272599835542));
#15116=CARTESIAN_POINT('Ctrl Pts',(-0.6646808418357,-3.977835246522,-2.276718416632));
#15117=CARTESIAN_POINT('Ctrl Pts',(1.002349255295,-4.115418579855,-2.149544914748));
#15118=CARTESIAN_POINT('Ctrl Pts',(2.171316101136,-4.253001913189,-0.9542713236204));
#15119=CARTESIAN_POINT('Ctrl Pts',(2.261364844106,-4.390585246522,0.715175790919));
#15120=CARTESIAN_POINT('Ctrl Pts',(1.227750631671,-4.528168579855,2.029254975732));
#15121=CARTESIAN_POINT('Ctrl Pts',(-0.4159278556647,-4.665751913189,2.335005650883));
#15122=CARTESIAN_POINT('Ctrl Pts',(-1.852933489305,-4.803335246522,1.480501553815));
#15123=CARTESIAN_POINT('Ctrl Pts',(-2.369224042948,-4.940918579855,-0.1096577165763));
#15124=CARTESIAN_POINT('Ctrl Pts',(-1.708256833279,-5.078501913189,-1.645328524034));
#15125=CARTESIAN_POINT('Ctrl Pts',(-0.198463826226,-5.216085246522,-2.363442275497));
#15126=CARTESIAN_POINT('Ctrl Pts',(1.409945218843,-5.353668579855,-1.907171332278));
#15127=CARTESIAN_POINT('Ctrl Pts',(2.317757596199,-5.491251913189,-0.5032342968815));
#15128=CARTESIAN_POINT('Ctrl Pts',(2.073888103704,-5.628835246522,1.150756140208));
#15129=CARTESIAN_POINT('Ctrl Pts',(0.7995030738709,-5.766418579855,2.232946765546));
#15130=CARTESIAN_POINT('Ctrl Pts',(-0.872118147943,-5.904001913189,2.205572069566));
#15131=CARTESIAN_POINT('Ctrl Pts',(-2.110512896131,-6.041585246522,1.082344177464));
#15132=CARTESIAN_POINT('Ctrl Pts',(-2.299734136718,-6.179168579855,-0.5790191531922));
#15133=CARTESIAN_POINT('Ctrl Pts',(-1.665227699375,-6.270890802077,-1.493982811308));
#15134=CARTESIAN_POINT('Ctrl Pts',(-1.235253620718,-6.316751913189,-1.790602059871));
#15135=CARTESIAN_POINT('Ctrl Pts',(2.149561232942,-1.951996799872,-0.2031933613371));
#15136=CARTESIAN_POINT('Ctrl Pts',(2.198353692354,-1.997857910983,0.3129769432571));
#15137=CARTESIAN_POINT('Ctrl Pts',(1.907485731021,-2.089580133205,1.379166202239));
#15138=CARTESIAN_POINT('Ctrl Pts',(0.5235602335809,-2.227163466539,2.295245980444));
#15139=CARTESIAN_POINT('Ctrl Pts',(-1.120573343748,-2.364746799872,2.070265262769));
#15140=CARTESIAN_POINT('Ctrl Pts',(-2.20788436476,-2.502330133205,0.8167288166584));
#15141=CARTESIAN_POINT('Ctrl Pts',(-2.198110477214,-2.639913466539,-0.842677202864));
#15142=CARTESIAN_POINT('Ctrl Pts',(-1.096103448508,-2.777496799872,-2.083349547407));
#15143=CARTESIAN_POINT('Ctrl Pts',(0.5505526332874,-2.915080133205,-2.2888169081));
#15144=CARTESIAN_POINT('Ctrl Pts',(1.923641433491,-3.052663466539,-1.3569797184));
#15145=CARTESIAN_POINT('Ctrl Pts',(2.340880642008,-3.190246799872,0.2491349433296));
#15146=CARTESIAN_POINT('Ctrl Pts',(1.594945825095,-3.327830133205,1.731455524949));
#15147=CARTESIAN_POINT('Ctrl Pts',(0.05648894014665,-3.465413466539,2.353422912665));
#15148=CARTESIAN_POINT('Ctrl Pts',(-1.510037068078,-3.602996799872,1.805984070618));
#15149=CARTESIAN_POINT('Ctrl Pts',(-2.326231824369,-3.740580133205,0.3611591185692));
#15150=CARTESIAN_POINT('Ctrl Pts',(-1.986531487591,-3.878163466539,-1.263124324211));
#15151=CARTESIAN_POINT('Ctrl Pts',(-0.6597317677654,-4.015746799872,-2.259766449053));
#15152=CARTESIAN_POINT('Ctrl Pts',(0.9948859730751,-4.153330133205,-2.133539854377));
#15153=CARTESIAN_POINT('Ctrl Pts',(2.15514893708,-4.290913466539,-0.9471660195909));
#15154=CARTESIAN_POINT('Ctrl Pts',(2.244527196006,-4.428496799872,0.7098507420537));
#15155=CARTESIAN_POINT('Ctrl Pts',(1.218609058101,-4.566080133205,2.014145569006));
#15156=CARTESIAN_POINT('Ctrl Pts',(-0.4128309441306,-4.703663466539,2.317619688789));
#15157=CARTESIAN_POINT('Ctrl Pts',(-1.839136935367,-4.841246799872,1.469478049916));
#15158=CARTESIAN_POINT('Ctrl Pts',(-2.351583297887,-4.978830133205,-0.1088412282295));
#15159=CARTESIAN_POINT('Ctrl Pts',(-1.695537511362,-5.116413466539,-1.633077753103));
#15160=CARTESIAN_POINT('Ctrl Pts',(-0.196986106222,-5.253996799872,-2.345844580263));
#15161=CARTESIAN_POINT('Ctrl Pts',(1.39944706261,-5.391580133205,-1.892970934742));
#15162=CARTESIAN_POINT('Ctrl Pts',(2.300500059501,-5.529163466539,-0.4994873199066));
#15163=CARTESIAN_POINT('Ctrl Pts',(2.058446368072,-5.666746799872,1.142187851465));
#15164=CARTESIAN_POINT('Ctrl Pts',(0.7935501417522,-5.804330133205,2.216320712496));
#15165=CARTESIAN_POINT('Ctrl Pts',(-0.8656245392205,-5.941913466539,2.189149842758));
#15166=CARTESIAN_POINT('Ctrl Pts',(-2.094798459981,-6.079496799872,1.07428526984));
#15167=CARTESIAN_POINT('Ctrl Pts',(-2.282610798917,-6.217080133205,-0.5747078980801));
#15168=CARTESIAN_POINT('Ctrl Pts',(-1.652828763361,-6.308802355428,-1.482858928795));
#15169=CARTESIAN_POINT('Ctrl Pts',(-1.226056181467,-6.354663466539,-1.777269612677));
#15170=CARTESIAN_POINT('Ctrl Pts',(2.10063415235,-2.166998399936,-0.1985683905227));
#15171=CARTESIAN_POINT('Ctrl Pts',(2.14831602577,-2.212859511047,0.3058531414823));
#15172=CARTESIAN_POINT('Ctrl Pts',(1.864068634239,-2.304581733269,1.347774411722));
#15173=CARTESIAN_POINT('Ctrl Pts',(0.5116432556643,-2.442165066603,2.24300290714));
#15174=CARTESIAN_POINT('Ctrl Pts',(-1.095067495643,-2.579748399936,2.023143071595));
#15175=CARTESIAN_POINT('Ctrl Pts',(-2.157629766474,-2.717331733269,0.7981389035067));
#15176=CARTESIAN_POINT('Ctrl Pts',(-2.148078346554,-2.854915066603,-0.8234966674198));
#15177=CARTESIAN_POINT('Ctrl Pts',(-1.071154570131,-2.992498399936,-2.035929539246));
#15178=CARTESIAN_POINT('Ctrl Pts',(0.5380212698415,-3.130081733269,-2.236720169656));
#15179=CARTESIAN_POINT('Ctrl Pts',(1.87985660987,-3.267665066603,-1.326092923911));
#15180=CARTESIAN_POINT('Ctrl Pts',(2.287598858697,-3.405248399936,0.2434642765611));
#15181=CARTESIAN_POINT('Ctrl Pts',(1.558642582494,-3.542831733269,1.692045126811));
#15182=CARTESIAN_POINT('Ctrl Pts',(0.05520317127216,-3.680415066603,2.299855649378));
#15183=CARTESIAN_POINT('Ctrl Pts',(-1.475666469932,-3.817998399936,1.764877296446));
#15184=CARTESIAN_POINT('Ctrl Pts',(-2.273283469047,-3.955581733269,0.3529386217393));
#15185=CARTESIAN_POINT('Ctrl Pts',(-1.941315196609,-4.093165066603,-1.234373812404));
#15186=CARTESIAN_POINT('Ctrl Pts',(-0.6447153314452,-4.230748399936,-2.208330940504));
#15187=CARTESIAN_POINT('Ctrl Pts',(0.972240948854,-4.368331733269,-2.08497744322));
#15188=CARTESIAN_POINT('Ctrl Pts',(2.106094672369,-4.505915066603,-0.9256071695965));
#15189=CARTESIAN_POINT('Ctrl Pts',(2.1934385546,-4.643498399936,0.6936935263705));
#15190=CARTESIAN_POINT('Ctrl Pts',(1.190871777263,-4.781081733269,1.968300742132));
#15191=CARTESIAN_POINT('Ctrl Pts',(-0.4034343228272,-4.918665066603,2.264867357961));
#15192=CARTESIAN_POINT('Ctrl Pts',(-1.797275554691,-5.056248399936,1.436030632892));
#15193=CARTESIAN_POINT('Ctrl Pts',(-2.298057906858,-5.193831733269,-0.1063638465836));
#15194=CARTESIAN_POINT('Ctrl Pts',(-1.656944658461,-5.331415066603,-1.595906573415));
#15195=CARTESIAN_POINT('Ctrl Pts',(-0.1925024213904,-5.468998399936,-2.292449810634));
#15196=CARTESIAN_POINT('Ctrl Pts',(1.367593650775,-5.606581733269,-1.849884215432));
#15197=CARTESIAN_POINT('Ctrl Pts',(2.248137395861,-5.744165066603,-0.4881182758517));
#15198=CARTESIAN_POINT('Ctrl Pts',(2.011593191805,-5.881748399936,1.116190026326));
#15199=CARTESIAN_POINT('Ctrl Pts',(0.775487808312,-6.019331733269,2.165874090898));
#15200=CARTESIAN_POINT('Ctrl Pts',(-0.8459216896603,-6.156915066603,2.139321668922));
#15201=CARTESIAN_POINT('Ctrl Pts',(-2.047117858235,-6.294498399936,1.04983300434));
#15202=CARTESIAN_POINT('Ctrl Pts',(-2.230655320372,-6.432081733269,-0.5616267263435));
#15203=CARTESIAN_POINT('Ctrl Pts',(-1.615208022499,-6.523803955492,-1.449106943876));
#15204=CARTESIAN_POINT('Ctrl Pts',(-1.198149393476,-6.569665066603,-1.736816420537));
#15205=CARTESIAN_POINT('Ctrl Pts',(2.488904911508,-2.557,-0.2352707832963));
#15206=CARTESIAN_POINT('Ctrl Pts',(2.545400065037,-2.602861111111,0.3623855135288));
#15207=CARTESIAN_POINT('Ctrl Pts',(2.208613800721,-2.694583333333,1.596890324375));
#15208=CARTESIAN_POINT('Ctrl Pts',(0.6062128479337,-2.832166666667,2.657588398181));
#15209=CARTESIAN_POINT('Ctrl Pts',(-1.297474319976,-2.96975,2.397090765159));
#15210=CARTESIAN_POINT('Ctrl Pts',(-2.556435311206,-3.107333333333,0.9456629250653));
#15211=CARTESIAN_POINT('Ctrl Pts',(-2.545118454378,-3.244916666667,-0.9757076918219));
#15212=CARTESIAN_POINT('Ctrl Pts',(-1.269141448358,-3.3825,-2.412240619837));
#15213=CARTESIAN_POINT('Ctrl Pts',(0.6374664429341,-3.520083333333,-2.650144390777));
#15214=CARTESIAN_POINT('Ctrl Pts',(2.22731994717,-3.657666666667,-1.571201338294));
#15215=CARTESIAN_POINT('Ctrl Pts',(2.710427243412,-3.79525,0.2884650014053));
#15216=CARTESIAN_POINT('Ctrl Pts',(1.846734318071,-3.932833333333,2.004794324563));
#15217=CARTESIAN_POINT('Ctrl Pts',(0.06540665063283,-4.070416666667,2.724949518265));
#15218=CARTESIAN_POINT('Ctrl Pts',(-1.748421313941,-4.208,2.091088429853));
#15219=CARTESIAN_POINT('Ctrl Pts',(-2.693465868406,-4.345583333333,0.4181740395515));
#15220=CARTESIAN_POINT('Ctrl Pts',(-2.300138233124,-4.483166666667,-1.46252932282));
#15221=CARTESIAN_POINT('Ctrl Pts',(-0.7638813037308,-4.62075,-2.616507837839));
#15222=CARTESIAN_POINT('Ctrl Pts',(1.151945125744,-4.758333333333,-2.470354294206));
#15223=CARTESIAN_POINT('Ctrl Pts',(2.495374726863,-4.895916666667,-1.096691790885));
#15224=CARTESIAN_POINT('Ctrl Pts',(2.598862817463,-5.0335,0.8219123843785));
#15225=CARTESIAN_POINT('Ctrl Pts',(1.41098658807,-5.171083333333,2.332111652539));
#15226=CARTESIAN_POINT('Ctrl Pts',(-0.4780031146462,-5.308666666667,2.683494165244));
#15227=CARTESIAN_POINT('Ctrl Pts',(-2.129475020865,-5.44625,1.701459386102));
#15228=CARTESIAN_POINT('Ctrl Pts',(-2.722819489967,-5.583833333333,-0.1260236104762));
#15229=CARTESIAN_POINT('Ctrl Pts',(-1.963206060383,-5.721416666667,-1.890885999562));
#15230=CARTESIAN_POINT('Ctrl Pts',(-0.2280836106277,-5.859,-2.716174821156));
#15231=CARTESIAN_POINT('Ctrl Pts',(1.620372852909,-5.996583333333,-2.191807604556));
#15232=CARTESIAN_POINT('Ctrl Pts',(2.663671920236,-6.134166666667,-0.5783396279667));
#15233=CARTESIAN_POINT('Ctrl Pts',(2.383406063087,-6.27175,1.322501034076));
#15234=CARTESIAN_POINT('Ctrl Pts',(0.9188251141986,-6.409333333333,2.566203475515));
#15235=CARTESIAN_POINT('Ctrl Pts',(-1.002277643535,-6.546916666667,2.534743236046));
#15236=CARTESIAN_POINT('Ctrl Pts',(-2.425496932009,-6.6845,1.243878910491));
#15237=CARTESIAN_POINT('Ctrl Pts',(-2.642958544944,-6.822083333333,-0.6654350145011));
#15238=CARTESIAN_POINT('Ctrl Pts',(-1.913755032407,-6.913805555556,-1.71695265731));
#15239=CARTESIAN_POINT('Ctrl Pts',(-1.419609362633,-6.959666666667,-2.057840921336));
#15240=CARTESIAN_POINT('Ctrl Pts',(2.877175670666,-2.166998399936,-0.2719731760698));
#15241=CARTESIAN_POINT('Ctrl Pts',(2.942484104304,-2.212859511047,0.4189178855753));
#15242=CARTESIAN_POINT('Ctrl Pts',(2.553158967202,-2.304581733269,1.846006237029));
#15243=CARTESIAN_POINT('Ctrl Pts',(0.700782440203,-2.442165066603,3.072173889222));
#15244=CARTESIAN_POINT('Ctrl Pts',(-1.499881144309,-2.579748399936,2.771038458724));
#15245=CARTESIAN_POINT('Ctrl Pts',(-2.955240855938,-2.717331733269,1.093186946624));
#15246=CARTESIAN_POINT('Ctrl Pts',(-2.942158562201,-2.854915066603,-1.127918716224));
#15247=CARTESIAN_POINT('Ctrl Pts',(-1.467128326585,-2.992498399936,-2.788551700427));
#15248=CARTESIAN_POINT('Ctrl Pts',(0.7369116160266,-3.130081733269,-3.063568611899));
#15249=CARTESIAN_POINT('Ctrl Pts',(2.574783284471,-3.267665066603,-1.816309752677));
#15250=CARTESIAN_POINT('Ctrl Pts',(3.133255628127,-3.405248399936,0.3334657262495));
#15251=CARTESIAN_POINT('Ctrl Pts',(2.134826053647,-3.542831733269,2.317543522314));
#15252=CARTESIAN_POINT('Ctrl Pts',(0.07561012999347,-3.680415066603,3.150043387152));
#15253=CARTESIAN_POINT('Ctrl Pts',(-2.02117615795,-3.817998399936,2.41729956326));
#15254=CARTESIAN_POINT('Ctrl Pts',(-3.113648267764,-3.955581733269,0.4834094573636));
#15255=CARTESIAN_POINT('Ctrl Pts',(-2.658961269639,-4.093165066603,-1.690684833236));
#15256=CARTESIAN_POINT('Ctrl Pts',(-0.8830472760164,-4.230748399936,-3.024684735174));
#15257=CARTESIAN_POINT('Ctrl Pts',(1.331649302635,-4.368331733269,-2.855731145192));
#15258=CARTESIAN_POINT('Ctrl Pts',(2.884654781358,-4.505915066603,-1.267776412174));
#15259=CARTESIAN_POINT('Ctrl Pts',(3.004287080326,-4.643498399936,0.9501312423865));
#15260=CARTESIAN_POINT('Ctrl Pts',(1.631101398876,-4.781081733269,2.695922562946));
#15261=CARTESIAN_POINT('Ctrl Pts',(-0.5525719064653,-4.918665066603,3.102120972527));
#15262=CARTESIAN_POINT('Ctrl Pts',(-2.461674487038,-5.056248399936,1.966888139311));
#15263=CARTESIAN_POINT('Ctrl Pts',(-3.147581073076,-5.193831733269,-0.1456833743688));
#15264=CARTESIAN_POINT('Ctrl Pts',(-2.269467462304,-5.331415066603,-2.185865425709));
#15265=CARTESIAN_POINT('Ctrl Pts',(-0.263664799865,-5.468998399936,-3.139899831678));
#15266=CARTESIAN_POINT('Ctrl Pts',(1.873152055043,-5.606581733269,-2.53373099368));
#15267=CARTESIAN_POINT('Ctrl Pts',(3.079206444611,-5.744165066603,-0.6685609800817));
#15268=CARTESIAN_POINT('Ctrl Pts',(2.755218934369,-5.881748399936,1.528812041827));
#15269=CARTESIAN_POINT('Ctrl Pts',(1.062162420085,-6.019331733269,2.966532860131));
#15270=CARTESIAN_POINT('Ctrl Pts',(-1.15863359741,-6.156915066603,2.930164803169));
#15271=CARTESIAN_POINT('Ctrl Pts',(-2.803876005782,-6.294498399936,1.437924816642));
#15272=CARTESIAN_POINT('Ctrl Pts',(-3.055261769517,-6.432081733269,-0.7692433026587));
#15273=CARTESIAN_POINT('Ctrl Pts',(-2.212302042314,-6.523803955492,-1.984798370744));
#15274=CARTESIAN_POINT('Ctrl Pts',(-1.64106933179,-6.569665066603,-2.378865422135));
#15275=CARTESIAN_POINT('Ctrl Pts',(2.828248590073,-1.951996799872,-0.2673482052555));
#15276=CARTESIAN_POINT('Ctrl Pts',(2.89244643772,-1.997857910983,0.4117940838004));
#15277=CARTESIAN_POINT('Ctrl Pts',(2.50974187042,-2.089580133205,1.814614446512));
#15278=CARTESIAN_POINT('Ctrl Pts',(0.6888654622864,-2.227163466539,3.019930815918));
#15279=CARTESIAN_POINT('Ctrl Pts',(-1.474375296204,-2.364746799872,2.72391626755));
#15280=CARTESIAN_POINT('Ctrl Pts',(-2.904986257652,-2.502330133205,1.074597033472));
#15281=CARTESIAN_POINT('Ctrl Pts',(-2.892126431541,-2.639913466539,-1.10873818078));
#15282=CARTESIAN_POINT('Ctrl Pts',(-1.442179448209,-2.777496799872,-2.741131692266));
#15283=CARTESIAN_POINT('Ctrl Pts',(0.7243802525807,-2.915080133205,-3.011471873454));
#15284=CARTESIAN_POINT('Ctrl Pts',(2.53099846085,-3.052663466539,-1.785422958187));
#15285=CARTESIAN_POINT('Ctrl Pts',(3.079973844815,-3.190246799872,0.3277950594809));
#15286=CARTESIAN_POINT('Ctrl Pts',(2.098522811046,-3.327830133205,2.278133124177));
#15287=CARTESIAN_POINT('Ctrl Pts',(0.07432436111898,-3.465413466539,3.096476123865));
#15288=CARTESIAN_POINT('Ctrl Pts',(-1.986805559805,-3.602996799872,2.376192789088));
#15289=CARTESIAN_POINT('Ctrl Pts',(-3.060699912442,-3.740580133205,0.4751889605338));
#15290=CARTESIAN_POINT('Ctrl Pts',(-2.613744978657,-3.878163466539,-1.661934321428));
#15291=CARTESIAN_POINT('Ctrl Pts',(-0.8680308396962,-4.015746799872,-2.973249226626));
#15292=CARTESIAN_POINT('Ctrl Pts',(1.309004278414,-4.153330133205,-2.807168734035));
#15293=CARTESIAN_POINT('Ctrl Pts',(2.835600516647,-4.290913466539,-1.24621756218));
#15294=CARTESIAN_POINT('Ctrl Pts',(2.95319843892,-4.428496799872,0.9339740267032));
#15295=CARTESIAN_POINT('Ctrl Pts',(1.603364118038,-4.566080133205,2.650077736072));
#15296=CARTESIAN_POINT('Ctrl Pts',(-0.5431752851618,-4.703663466539,3.049368641699));
#15297=CARTESIAN_POINT('Ctrl Pts',(-2.419813106363,-4.841246799872,1.933440722287));
#15298=CARTESIAN_POINT('Ctrl Pts',(-3.094055682046,-4.978830133205,-0.1432059927228));
#15299=CARTESIAN_POINT('Ctrl Pts',(-2.230874609403,-5.116413466539,-2.148694246022));
#15300=CARTESIAN_POINT('Ctrl Pts',(-0.2591811150334,-5.253996799872,-3.086505062049));
#15301=CARTESIAN_POINT('Ctrl Pts',(1.841298643208,-5.391580133205,-2.49064427437));
#15302=CARTESIAN_POINT('Ctrl Pts',(3.026843780971,-5.529163466539,-0.6571919360268));
#15303=CARTESIAN_POINT('Ctrl Pts',(2.708365758102,-5.666746799872,1.502814216688));
#15304=CARTESIAN_POINT('Ctrl Pts',(1.044100086645,-5.804330133205,2.916086238533));
#15305=CARTESIAN_POINT('Ctrl Pts',(-1.13893074785,-5.941913466539,2.880336629334));
#15306=CARTESIAN_POINT('Ctrl Pts',(-2.756195404036,-6.079496799872,1.413472551141));
#15307=CARTESIAN_POINT('Ctrl Pts',(-3.003306290972,-6.217080133205,-0.7561621309221));
#15308=CARTESIAN_POINT('Ctrl Pts',(-2.174681301453,-6.308802355428,-1.951046385826));
#15309=CARTESIAN_POINT('Ctrl Pts',(-1.613162543799,-6.354663466539,-2.338412229995));
#15310=CARTESIAN_POINT('Ctrl Pts',(2.812123342995,-1.914085246522,-0.265823920622));
#15311=CARTESIAN_POINT('Ctrl Pts',(2.875955166892,-1.959946357633,0.4094462416164));
#15312=CARTESIAN_POINT('Ctrl Pts',(2.495432588024,-2.051668579855,1.80426843011));
#15313=CARTESIAN_POINT('Ctrl Pts',(0.6849378988389,-2.189251913189,3.00271269346));
#15314=CARTESIAN_POINT('Ctrl Pts',(-1.465969151843,-2.326835246522,2.708385870756));
#15315=CARTESIAN_POINT('Ctrl Pts',(-2.888423491095,-2.464418579855,1.068470223143));
#15316=CARTESIAN_POINT('Ctrl Pts',(-2.875636985226,-2.602001913189,-1.102416714848));
#15317=CARTESIAN_POINT('Ctrl Pts',(-1.433956868336,-2.739585246522,-2.725503141803));
#15318=CARTESIAN_POINT('Ctrl Pts',(0.7202502017102,-2.877168579855,-2.994301979619));
#15319=CARTESIAN_POINT('Ctrl Pts',(2.516567984095,-3.014751913189,-1.775243376929));
#15320=CARTESIAN_POINT('Ctrl Pts',(3.062413387288,-3.152335246522,0.32592613737));
#15321=CARTESIAN_POINT('Ctrl Pts',(2.086558092334,-3.289918579855,2.265144358043));
#15322=CARTESIAN_POINT('Ctrl Pts',(0.07390060109619,-3.427501913189,3.078821578666));
#15323=CARTESIAN_POINT('Ctrl Pts',(-1.975477796517,-3.565085246522,2.3626449362));
#15324=CARTESIAN_POINT('Ctrl Pts',(-3.043249345157,-3.702668579855,0.4724796727348));
#15325=CARTESIAN_POINT('Ctrl Pts',(-2.598842722989,-3.840251913189,-1.652458810098));
#15326=CARTESIAN_POINT('Ctrl Pts',(-0.8630817656259,-3.977835246522,-2.956297259047));
#15327=CARTESIAN_POINT('Ctrl Pts',(1.301540996194,-4.115418579855,-2.791163673665));
#15328=CARTESIAN_POINT('Ctrl Pts',(2.819433352591,-4.253001913189,-1.239112258151));
#15329=CARTESIAN_POINT('Ctrl Pts',(2.93636079082,-4.390585246522,0.928648977838));
#15330=CARTESIAN_POINT('Ctrl Pts',(1.594222544469,-4.528168579855,2.634968329346));
#15331=CARTESIAN_POINT('Ctrl Pts',(-0.5400783736277,-4.665751913189,3.031982679605));
#15332=CARTESIAN_POINT('Ctrl Pts',(-2.406016552425,-4.803335246522,1.922417218389));
#15333=CARTESIAN_POINT('Ctrl Pts',(-3.076414936985,-4.940918579855,-0.142389504376));
#15334=CARTESIAN_POINT('Ctrl Pts',(-2.218155287486,-5.078501913189,-2.136443475091));
#15335=CARTESIAN_POINT('Ctrl Pts',(-0.2577033950294,-5.216085246522,-3.068907366815));
#15336=CARTESIAN_POINT('Ctrl Pts',(1.830800486974,-5.353668579855,-2.476443876835));
#15337=CARTESIAN_POINT('Ctrl Pts',(3.009586244273,-5.491251913189,-0.653444959052));
#15338=CARTESIAN_POINT('Ctrl Pts',(2.69292402247,-5.628835246522,1.494245927945));
#15339=CARTESIAN_POINT('Ctrl Pts',(1.038147154526,-5.766418579855,2.899460185483));
#15340=CARTESIAN_POINT('Ctrl Pts',(-1.132437139127,-5.904001913189,2.863914402526));
#15341=CARTESIAN_POINT('Ctrl Pts',(-2.740480967886,-6.041585246522,1.405413643517));
#15342=CARTESIAN_POINT('Ctrl Pts',(-2.98618295317,-6.179168579855,-0.75185087581));
#15343=CARTESIAN_POINT('Ctrl Pts',(-2.162282365438,-6.270890802077,-1.939922503313));
#15344=CARTESIAN_POINT('Ctrl Pts',(-1.603965104547,-6.316751913189,-2.325079782801));
#15345=CARTESIAN_POINT('',(-2.46657190792704,-6.35000032196109,-1.42407460247911));
#15346=CARTESIAN_POINT('Ctrl Pts',(2.67638549957928,-2.11666634473297,0.974128396786123));
#15347=CARTESIAN_POINT('Ctrl Pts',(2.63158429467461,-2.1254957760933,1.09794595690002));
#15348=CARTESIAN_POINT('Ctrl Pts',(2.57832130571527,-2.13432523104768,1.21881530794275));
#15349=CARTESIAN_POINT('Ctrl Pts',(2.51693294178586,-2.14315470006068,1.33539535663631));
#15350=CARTESIAN_POINT('Ctrl Pts',(2.45569542878568,-2.15196247223212,1.45168893070262));
#15351=CARTESIAN_POINT('Ctrl Pts',(2.38637276527163,-2.16077025839314,1.56371307377647));
#15352=CARTESIAN_POINT('Ctrl Pts',(2.30934763707904,-2.16957804907858,1.67015373268866));
#15353=CARTESIAN_POINT('Ctrl Pts',(2.2544280617514,-2.17585807918525,1.74604683306021));
#15354=CARTESIAN_POINT('Ctrl Pts',(2.19559382630051,-2.18213811159205,1.81910178374938));
#15355=CARTESIAN_POINT('Ctrl Pts',(2.1332634233653,-2.18841814286804,1.88903780308403));
#15356=CARTESIAN_POINT('Ctrl Pts',(2.04207818376161,-2.19760541151469,1.99134955432665));
#15357=CARTESIAN_POINT('Ctrl Pts',(1.94345554311775,-2.20679260757273,2.08694592181752));
#15358=CARTESIAN_POINT('Ctrl Pts',(1.83858684135808,-2.21597977160931,2.17511176619573));
#15359=CARTESIAN_POINT('Ctrl Pts',(1.73114043431015,-2.22539275899379,2.2654447544356));
#15360=CARTESIAN_POINT('Ctrl Pts',(1.61713621323921,-2.2348057127633,2.34797828870751));
#15361=CARTESIAN_POINT('Ctrl Pts',(1.49781311768319,-2.24421867655057,2.42190950106786));
#15362=CARTESIAN_POINT('Ctrl Pts',(1.43041393440689,-2.24953555228628,2.46366925686782));
#15363=CARTESIAN_POINT('Ctrl Pts',(1.36131707299677,-2.25485243121816,2.50268375528082));
#15364=CARTESIAN_POINT('Ctrl Pts',(1.29074180256227,-2.26016932120947,2.53880214744044));
#15365=CARTESIAN_POINT('Ctrl Pts',(1.17763832214355,-2.26869013536035,2.59668525345238));
#15366=CARTESIAN_POINT('Ctrl Pts',(1.06062583874571,-2.27721098490573,2.64718152713231));
#15367=CARTESIAN_POINT('Ctrl Pts',(0.940746669490456,-2.28573185613866,
2.68956035801277));
#15368=CARTESIAN_POINT('Ctrl Pts',(0.840248387944155,-2.29287515652609,
2.72508779538063));
#15369=CARTESIAN_POINT('Ctrl Pts',(0.737736391549633,-2.30001847215547,
2.75491074422656));
#15370=CARTESIAN_POINT('Ctrl Pts',(0.633838265760999,-2.307161794951,2.77862358958537));
#15371=CARTESIAN_POINT('Ctrl Pts',(0.513799258434475,-2.31541485409794,
2.80602029569679));
#15372=CARTESIAN_POINT('Ctrl Pts',(0.391910586283146,-2.32366792281057,
2.82525992132688));
#15373=CARTESIAN_POINT('Ctrl Pts',(0.269315413872178,-2.33192098863433,
2.83649454098679));
#15374=CARTESIAN_POINT('Ctrl Pts',(0.133629132011341,-2.3410553435486,2.84892882970954));
#15375=CARTESIAN_POINT('Ctrl Pts',(-0.0029017556927971,-2.35018960945232,
2.8515644826885));
#15376=CARTESIAN_POINT('Ctrl Pts',(-0.138944627445231,-2.35932384692222,
2.84464052964891));
#15377=CARTESIAN_POINT('Ctrl Pts',(-0.277065228126552,-2.36859758798529,
2.83761082981533));
#15378=CARTESIAN_POINT('Ctrl Pts',(-0.414684058841455,-2.37787129973941,
2.82072724303376));
#15379=CARTESIAN_POINT('Ctrl Pts',(-0.550411283063103,-2.38714504557935,
2.79418713351009));
#15380=CARTESIAN_POINT('Ctrl Pts',(-0.631039269717429,-2.39265406162315,
2.77842113218832));
#15381=CARTESIAN_POINT('Ctrl Pts',(-0.710999729177977,-2.39816308969545,
2.75924645530946));
#15382=CARTESIAN_POINT('Ctrl Pts',(-0.789999251472441,-2.40367214308581,
2.73669598970977));
#15383=CARTESIAN_POINT('Ctrl Pts',(-0.908818344442536,-2.41195802517665,
2.70277900147002));
#15384=CARTESIAN_POINT('Ctrl Pts',(-1.02554898172219,-2.42024391903388,
2.66119535121063));
#15385=CARTESIAN_POINT('Ctrl Pts',(-1.13901931890348,-2.42852982142298,
2.61208499993025));
#15386=CARTESIAN_POINT('Ctrl Pts',(-1.21304893126723,-2.43393565837726,
2.58004472968301));
#15387=CARTESIAN_POINT('Ctrl Pts',(-1.28569081934136,-2.43934149896308,
2.54480182943131));
#15388=CARTESIAN_POINT('Ctrl Pts',(-1.35662275119696,-2.44474734228225,
2.50640673292635));
#15389=CARTESIAN_POINT('Ctrl Pts',(-1.46519412681361,-2.45302175170798,
2.44763759559389));
#15390=CARTESIAN_POINT('Ctrl Pts',(-1.56975749516473,-2.46129616753761,
2.38148148479742));
#15391=CARTESIAN_POINT('Ctrl Pts',(-1.66953923951437,-2.46957058655012,
2.30881919414378));
#15392=CARTESIAN_POINT('Ctrl Pts',(-1.69306756156468,-2.47152167686804,
2.29168558131155));
#15393=CARTESIAN_POINT('Ctrl Pts',(-1.71633016792867,-2.47347276736293,
2.2741903971365));
#15394=CARTESIAN_POINT('Ctrl Pts',(-1.73931720410331,-2.47542385799256,
2.25634549413614));
#15395=CARTESIAN_POINT('Ctrl Pts',(-1.8460242040886,-2.48448092068674,2.17350853987499));
#15396=CARTESIAN_POINT('Ctrl Pts',(-1.9468210578866,-2.4935378834916,2.08311981244695));
#15397=CARTESIAN_POINT('Ctrl Pts',(-2.04088398830876,-2.50259482028277,
1.98619769337065));
#15398=CARTESIAN_POINT('Ctrl Pts',(-2.13553289721494,-2.51170817855758,
1.88867178408551));
#15399=CARTESIAN_POINT('Ctrl Pts',(-2.22336458635848,-2.52082151049358,
1.78452990498833));
#15400=CARTESIAN_POINT('Ctrl Pts',(-2.30350597793839,-2.5299348913556,1.67477021328633));
#15401=CARTESIAN_POINT('Ctrl Pts',(-2.35404114510278,-2.53568156253532,
1.60555848313385));
#15402=CARTESIAN_POINT('Ctrl Pts',(-2.40151773977062,-2.54142825316924,
1.53411223130499));
#15403=CARTESIAN_POINT('Ctrl Pts',(-2.44570763150553,-2.54717498212873,
1.46067629080571));
#15404=CARTESIAN_POINT('Ctrl Pts',(-2.50880633543785,-2.55538073088615,
1.35581718195448));
#15405=CARTESIAN_POINT('Ctrl Pts',(-2.56522751641537,-2.56358647960479,
1.24685081219773));
#15406=CARTESIAN_POINT('Ctrl Pts',(-2.61420861752981,-2.57179222757394,
1.1346374093582));
#15407=CARTESIAN_POINT('Ctrl Pts',(-2.63518312611563,-2.57530606305979,
1.08658579500589));
#15408=CARTESIAN_POINT('Ctrl Pts',(-2.65479386158097,-2.57881989840821,
1.03793917153882));
#15409=CARTESIAN_POINT('Ctrl Pts',(-2.67298346364342,-2.58233373356339,
0.988766606983592));
#15410=CARTESIAN_POINT('Ctrl Pts',(-2.71546996183929,-2.59054120014066,
0.873911423891086));
#15411=CARTESIAN_POINT('Ctrl Pts',(-2.75019953557524,-2.59874866566371,
0.756186135019429));
#15412=CARTESIAN_POINT('Ctrl Pts',(-2.77716835857481,-2.60695612942142,
0.636738152390488));
#15413=CARTESIAN_POINT('Ctrl Pts',(-2.7902797066403,-2.61094632632634,0.578666501432876));
#15414=CARTESIAN_POINT('Ctrl Pts',(-2.80155751730202,-2.614936522814,0.520187858339262));
#15415=CARTESIAN_POINT('Ctrl Pts',(-2.81100576722147,-2.61892671880269,
0.461434456263184));
#15416=CARTESIAN_POINT('Ctrl Pts',(-2.83257209637234,-2.62803463622678,
0.327325471137989));
#15417=CARTESIAN_POINT('Ctrl Pts',(-2.84462417066588,-2.63714246177211,
0.191708380271717));
#15418=CARTESIAN_POINT('Ctrl Pts',(-2.84720452032045,-2.64625026874975,
0.0559117117292025));
#15419=CARTESIAN_POINT('Ctrl Pts',(-2.84977909096886,-2.65533767768847,
-0.0795808236956612));
#15420=CARTESIAN_POINT('Ctrl Pts',(-2.84292428703749,-2.66442506814257,
-0.215253398492207));
#15421=CARTESIAN_POINT('Ctrl Pts',(-2.8266315877823,-2.67351251293159,-0.349789492086304));
#15422=CARTESIAN_POINT('Ctrl Pts',(-2.81637317564084,-2.67923426305405,
-0.434497782245832));
#15423=CARTESIAN_POINT('Ctrl Pts',(-2.80237222267494,-2.6849560347169,-0.518755526343385));
#15424=CARTESIAN_POINT('Ctrl Pts',(-2.78461630087962,-2.69067784609661,
-0.602231317561455));
#15425=CARTESIAN_POINT('Ctrl Pts',(-2.75885578422968,-2.69897912265177,
-0.723339054705511));
#15426=CARTESIAN_POINT('Ctrl Pts',(-2.72518225862423,-2.70728039666944,
-0.842816999871552));
#15427=CARTESIAN_POINT('Ctrl Pts',(-2.68360003639548,-2.71558166376684,
-0.959480990643439));
#15428=CARTESIAN_POINT('Ctrl Pts',(-2.67635637108904,-2.71702775291864,
-0.979803976216825));
#15429=CARTESIAN_POINT('Ctrl Pts',(-2.66887283467555,-2.71847384186044,
-1.00004159014573));
#15430=CARTESIAN_POINT('Ctrl Pts',(-2.6611496096252,-2.71991993056907,-1.02018760778401));
#15431=CARTESIAN_POINT('Ctrl Pts',(-2.61673255514137,-2.72823653413051,
-1.13604940868169));
#15432=CARTESIAN_POINT('Ctrl Pts',(-2.56438391160144,-2.73655312997981,
-1.24887965301854));
#15433=CARTESIAN_POINT('Ctrl Pts',(-2.50488242176999,-2.74486971370987,
-1.35778164951388));
#15434=CARTESIAN_POINT('Ctrl Pts',(-2.46300472313212,-2.75072300222636,
-1.43442788145216));
#15435=CARTESIAN_POINT('Ctrl Pts',(-2.41758499103118,-2.7565762847396,-1.50912864719515));
#15436=CARTESIAN_POINT('Ctrl Pts',(-2.3689070842741,-2.76242955971315,-1.58158059804684));
#15437=CARTESIAN_POINT('Ctrl Pts',(-2.29156242541089,-2.77172986833818,
-1.69669999811805));
#15438=CARTESIAN_POINT('Ctrl Pts',(-2.20593010819929,-2.78103011048508,
-1.80624681857931));
#15439=CARTESIAN_POINT('Ctrl Pts',(-2.11296872096421,-2.79033034681067,
-1.9091751950852));
#15440=CARTESIAN_POINT('Ctrl Pts',(-2.02106806477434,-2.79952446327627,
-2.01092911273627));
#15441=CARTESIAN_POINT('Ctrl Pts',(-1.92200373022194,-2.80871857405262,
-2.10621564516073));
#15442=CARTESIAN_POINT('Ctrl Pts',(-1.81666548897215,-2.81791273774381,
-2.19399031980656));
#15443=CARTESIAN_POINT('Ctrl Pts',(-1.75453793015004,-2.82333537380425,
-2.24575904308739));
#15444=CARTESIAN_POINT('Ctrl Pts',(-1.69022734883333,-2.8287580282713,-2.29491403170352));
#15445=CARTESIAN_POINT('Ctrl Pts',(-1.62391216664702,-2.83418071316825,
-2.3412334732007));
#15446=CARTESIAN_POINT('Ctrl Pts',(-1.52883304313051,-2.84195546564739,
-2.40764378459746));
#15447=CARTESIAN_POINT('Ctrl Pts',(-1.42964894747358,-2.84973022034248,
-2.46820934176147));
#15448=CARTESIAN_POINT('Ctrl Pts',(-1.32700138290461,-2.85750496714164,
-2.52221476672808));
#15449=CARTESIAN_POINT('Ctrl Pts',(-1.21336288402553,-2.86611219088953,
-2.58200279433791));
#15450=CARTESIAN_POINT('Ctrl Pts',(-1.09547996868788,-2.87471940496007,
-2.63374940496428));
#15451=CARTESIAN_POINT('Ctrl Pts',(-0.974642740719075,-2.88332659563305,
-2.67727993579873));
#15452=CARTESIAN_POINT('Ctrl Pts',(-0.868854144173173,-2.89086187790328,
-2.71538933172979));
#15453=CARTESIAN_POINT('Ctrl Pts',(-0.760802169834941,-2.89839714224074,
-2.74720229870293));
#15454=CARTESIAN_POINT('Ctrl Pts',(-0.651358559006033,-2.90593237943932,
-2.77263384914226));
#15455=CARTESIAN_POINT('Ctrl Pts',(-0.511049236294445,-2.91559273347731,
-2.80523770413774));
#15456=CARTESIAN_POINT('Ctrl Pts',(-0.368294800260247,-2.92525306083563,
-2.82739851538043));
#15457=CARTESIAN_POINT('Ctrl Pts',(-0.22468566984122,-2.93491339754972,
-2.83892488199066));
#15458=CARTESIAN_POINT('Ctrl Pts',(-0.0841848176923486,-2.94436464578452,
-2.85020177174127));
#15459=CARTESIAN_POINT('Ctrl Pts',(0.0571353952658782,-2.95381590297447,
-2.85129956142687));
#15460=CARTESIAN_POINT('Ctrl Pts',(0.197785017350908,-2.96326720286551,
-2.84199026349249));
#15461=CARTESIAN_POINT('Ctrl Pts',(0.269297302826939,-2.9680726480982,-2.83725701813004));
#15462=CARTESIAN_POINT('Ctrl Pts',(0.340636105777945,-2.97287810436972,
-2.82983260933662));
#15463=CARTESIAN_POINT('Ctrl Pts',(0.411603962273926,-2.97768357611561,
-2.81968208523217));
#15464=CARTESIAN_POINT('Ctrl Pts',(0.497282125125452,-2.98348513207562,
-2.80742754775295));
#15465=CARTESIAN_POINT('Ctrl Pts',(0.582386767266939,-2.98928669479688,
-2.79120315094139));
#15466=CARTESIAN_POINT('Ctrl Pts',(0.666528411393449,-2.99508825648647,
-2.77096370899068));
#15467=CARTESIAN_POINT('Ctrl Pts',(0.799366076867762,-3.00424740614358,
-2.73901091977262));
#15468=CARTESIAN_POINT('Ctrl Pts',(0.929802222571363,-3.01340655322936,
-2.69704856763171));
#15469=CARTESIAN_POINT('Ctrl Pts',(1.0565547050704,-3.02256566707968,-2.64593552148088));
#15470=CARTESIAN_POINT('Ctrl Pts',(1.18050383232203,-3.031522210934,-2.59595293071296));
#15471=CARTESIAN_POINT('Ctrl Pts',(1.30092953946802,-3.04047872300668,-2.53722077815605));
#15472=CARTESIAN_POINT('Ctrl Pts',(1.41665920877042,-3.04943517462354,-2.47058258696873));
#15473=CARTESIAN_POINT('Ctrl Pts',(1.54981361231564,-3.05974014637462,-2.39391107607299));
#15474=CARTESIAN_POINT('Ctrl Pts',(1.67693960457707,-3.07004514415773,-2.30667609351077));
#15475=CARTESIAN_POINT('Ctrl Pts',(1.79640033527703,-3.08035016642422,-2.20997267653908));
#15476=CARTESIAN_POINT('Ctrl Pts',(1.91175602400711,-3.09030107609944,-2.11659228951182));
#15477=CARTESIAN_POINT('Ctrl Pts',(2.0199650594349,-3.10025200860431,-2.01438211680193));
#15478=CARTESIAN_POINT('Ctrl Pts',(2.1195166720553,-3.11020296254449,-1.90429782257829));
#15479=CARTESIAN_POINT('Ctrl Pts',(2.15614367154787,-3.11386411453715,-1.86379564202554));
#15480=CARTESIAN_POINT('Ctrl Pts',(2.19159832758418,-3.1175252694314,-1.8222273436528));
#15481=CARTESIAN_POINT('Ctrl Pts',(2.2258037334462,-3.12118642715779,-1.77963979455017));
#15482=CARTESIAN_POINT('Ctrl Pts',(2.2615666211292,-3.1250142891363,-1.73511309776443));
#15483=CARTESIAN_POINT('Ctrl Pts',(2.29594976379294,-3.12884215682671,-1.68948953326672));
#15484=CARTESIAN_POINT('Ctrl Pts',(2.32886296023783,-3.13267002702334,-1.64283210107154));
#15485=CARTESIAN_POINT('Ctrl Pts',(2.41642064644769,-3.14285316004386,-1.51871116330901));
#15486=CARTESIAN_POINT('Ctrl Pts',(2.49357204651819,-3.15303631080089,-1.38727219520211));
#15487=CARTESIAN_POINT('Ctrl Pts',(2.55979938239103,-3.16321941894212,-1.25052854618166));
#15488=CARTESIAN_POINT('Ctrl Pts',(2.62422603598284,-3.17312565436676,-1.1175028764909));
#15489=CARTESIAN_POINT('Ctrl Pts',(2.67831448479832,-3.18303184946147,-0.979458378356245));
#15490=CARTESIAN_POINT('Ctrl Pts',(2.72163477731378,-3.19293794866419,-0.838256249921217));
#15491=CARTESIAN_POINT('Ctrl Pts',(2.77393013709443,-3.20489638642506,-0.667799965359726));
#15492=CARTESIAN_POINT('Ctrl Pts',(2.81063217923236,-3.21685492550503,-0.492454187357721));
#15493=CARTESIAN_POINT('Ctrl Pts',(2.83090292012302,-3.22881349999406,-0.315238782193383));
#15494=CARTESIAN_POINT('Ctrl Pts',(2.84943804737397,-3.23974816198248,-0.153196846811367));
#15495=CARTESIAN_POINT('Ctrl Pts',(2.85423479389205,-3.25068285357602,0.0104093356369592));
#15496=CARTESIAN_POINT('Ctrl Pts',(2.84460655496912,-3.26161752438638,0.17325672336415));
#15497=CARTESIAN_POINT('Ctrl Pts',(2.84370497481946,-3.26264143771307,0.188505615022862));
#15498=CARTESIAN_POINT('Ctrl Pts',(2.84267687832759,-3.26366535085753,0.203747835727151));
#15499=CARTESIAN_POINT('Ctrl Pts',(2.84152168048413,-3.26468926377839,0.218981466195257));
#15500=CARTESIAN_POINT('Ctrl Pts',(2.83942996306458,-3.26654326351079,0.246565009908956));
#15501=CARTESIAN_POINT('Ctrl Pts',(2.83692202091477,-3.26839726499412,0.274113823713482));
#15502=CARTESIAN_POINT('Ctrl Pts',(2.8339950153857,-3.27025126780648,0.301616068458823));
#15503=CARTESIAN_POINT('Ctrl Pts',(2.81452741727389,-3.28258229393223,0.484534290702154));
#15504=CARTESIAN_POINT('Ctrl Pts',(2.77651913214918,-3.2949133788493,0.66538988922194));
#15505=CARTESIAN_POINT('Ctrl Pts',(2.72163883591144,-3.30724439842938,0.840980151964874));
#15506=CARTESIAN_POINT('Ctrl Pts',(2.67832497503693,-3.31697656285171,0.97956344565591));
#15507=CARTESIAN_POINT('Ctrl Pts',(2.62450239319057,-3.32670868657539,1.11486715825269));
#15508=CARTESIAN_POINT('Ctrl Pts',(2.56100487279523,-3.33644070857623,1.24533559631229));
#15509=CARTESIAN_POINT('Ctrl Pts',(2.47221764009378,-3.35004878802035,1.42776683926587));
#15510=CARTESIAN_POINT('Ctrl Pts',(2.36434093956612,-3.36365705283171,1.60110913754079));
#15511=CARTESIAN_POINT('Ctrl Pts',(2.23940451281916,-3.37726534765327,1.76109550492112));
#15512=CARTESIAN_POINT('Ctrl Pts',(2.14585736922928,-3.38745466667601,1.88088657043688));
#15513=CARTESIAN_POINT('Ctrl Pts',(2.04274602578603,-3.39764400252361,1.99318890306528));
#15514=CARTESIAN_POINT('Ctrl Pts',(1.93092652160215,-3.40783328997986,2.09619244540513));
#15515=CARTESIAN_POINT('Ctrl Pts',(1.92961400303739,-3.40795289012516,2.09740148369003));
#15516=CARTESIAN_POINT('Ctrl Pts',(1.92830028473655,-3.4080724902638,2.09860924062003));
#15517=CARTESIAN_POINT('Ctrl Pts',(1.92698536963071,-3.40819209039566,2.09981571492913));
#15518=CARTESIAN_POINT('Ctrl Pts',(1.78095071869536,-3.42147489734707,2.23380691619397));
#15519=CARTESIAN_POINT('Ctrl Pts',(1.62042629665332,-3.43475778445623,2.35173263647907));
#15520=CARTESIAN_POINT('Ctrl Pts',(1.44955001995471,-3.44804061145149,2.45204164123285));
#15521=CARTESIAN_POINT('Ctrl Pts',(1.31274498852354,-3.45867495812436,2.53234990176673));
#15522=CARTESIAN_POINT('Ctrl Pts',(1.1693033470129,-3.46930926626579,2.60136638804764));
#15523=CARTESIAN_POINT('Ctrl Pts',(1.02132469790409,-3.47994346389266,2.65829384092901));
#15524=CARTESIAN_POINT('Ctrl Pts',(0.85476358086714,-3.49191305441258,2.72236997758179));
#15525=CARTESIAN_POINT('Ctrl Pts',(0.682161769008386,-3.50388279843517,
2.7712376313902));
#15526=CARTESIAN_POINT('Ctrl Pts',(0.506544247507313,-3.51585258313136,
2.80358587734168));
#15527=CARTESIAN_POINT('Ctrl Pts',(0.361966225971356,-3.52570676951775,
2.83021673603875));
#15528=CARTESIAN_POINT('Ctrl Pts',(0.215345706367376,-3.5355609834706,2.8456519610467));
#15529=CARTESIAN_POINT('Ctrl Pts',(0.0683885252654139,-3.54541516203575,
2.84917935721609));
#15530=CARTESIAN_POINT('Ctrl Pts',(0.0371714470076327,-3.54750841573814,
2.84992865712399));
#15531=CARTESIAN_POINT('Ctrl Pts',(0.00593921664234942,-3.54960166784371,
2.85014070352172));
#15532=CARTESIAN_POINT('Ctrl Pts',(-0.0252914674637119,-3.55169491774903,
2.84982099350694));
#15533=CARTESIAN_POINT('Ctrl Pts',(-0.185879903078349,-3.56245842605082,
2.84817704197036));
#15534=CARTESIAN_POINT('Ctrl Pts',(-0.34620802968348,-3.57322195383387,
2.83247981270469));
#15535=CARTESIAN_POINT('Ctrl Pts',(-0.504125026400352,-3.58398545793961,
2.8035682722057));
#15536=CARTESIAN_POINT('Ctrl Pts',(-0.670268236132065,-3.59530965455724,
2.77315067158857));
#15537=CARTESIAN_POINT('Ctrl Pts',(-0.833743800644653,-3.60663382496655,
2.72810615902489));
#15538=CARTESIAN_POINT('Ctrl Pts',(-0.992059497535025,-3.61795791890694,
2.66935668768567));
#15539=CARTESIAN_POINT('Ctrl Pts',(-1.0176358187225,-3.61978735635039,2.65986555460108));
#15540=CARTESIAN_POINT('Ctrl Pts',(-1.04307747231,-3.62161679179806,2.65001662193548));
#15541=CARTESIAN_POINT('Ctrl Pts',(-1.06837394293086,-3.62344622503802,
2.63981365250559));
#15542=CARTESIAN_POINT('Ctrl Pts',(-1.20691714936607,-3.63346562856756,
2.58393423275716));
#15543=CARTESIAN_POINT('Ctrl Pts',(-1.34129998177926,-3.64348512800569,
2.51735235049409));
#15544=CARTESIAN_POINT('Ctrl Pts',(-1.46963398238972,-3.65350466767422,
2.4406713441377));
#15545=CARTESIAN_POINT('Ctrl Pts',(-1.59554739801365,-3.66333522276206,
2.36543666449018));
#15546=CARTESIAN_POINT('Ctrl Pts',(-1.71563678789023,-3.67316581657696,
2.28048082016419));
#15547=CARTESIAN_POINT('Ctrl Pts',(-1.82813144995633,-3.68299639653218,
2.18642068265436));
#15548=CARTESIAN_POINT('Ctrl Pts',(-1.87467292357269,-3.687063519978,2.14750597036611));
#15549=CARTESIAN_POINT('Ctrl Pts',(-1.91991470040694,-3.69113064105153,
2.10703343267552));
#15550=CARTESIAN_POINT('Ctrl Pts',(-1.96379020164121,-3.69519775602884,
2.0651174806424));
#15551=CARTESIAN_POINT('Ctrl Pts',(-2.06986645150067,-3.70503067627827,
1.96377876368458));
#15552=CARTESIAN_POINT('Ctrl Pts',(-2.16785687873356,-3.7148635706403,1.85410545128513));
#15553=CARTESIAN_POINT('Ctrl Pts',(-2.25697365342708,-3.72469644251745,
1.73763937962582));
#15554=CARTESIAN_POINT('Ctrl Pts',(-2.34933317921239,-3.73488710961468,
1.61693537989596));
#15555=CARTESIAN_POINT('Ctrl Pts',(-2.4321623802172,-3.74507775256094,1.48893434178596));
#15556=CARTESIAN_POINT('Ctrl Pts',(-2.50455081037485,-3.75526837514386,
1.35530862510515));
#15557=CARTESIAN_POINT('Ctrl Pts',(-2.53220835593805,-3.7591619201177,1.30425406653183));
#15558=CARTESIAN_POINT('Ctrl Pts',(-2.55834136549607,-3.76305546211892,
1.25237805780557));
#15559=CARTESIAN_POINT('Ctrl Pts',(-2.58289742121862,-3.76694900135878,
1.19977273255586));
#15560=CARTESIAN_POINT('Ctrl Pts',(-2.6401218230586,-3.77602234182351,1.07718349000714));
#15561=CARTESIAN_POINT('Ctrl Pts',(-2.68884667112697,-3.78509574169171,
0.950484867996509));
#15562=CARTESIAN_POINT('Ctrl Pts',(-2.72829656318992,-3.79416917286518,
0.8209674215693));
#15563=CARTESIAN_POINT('Ctrl Pts',(-2.76657077212904,-3.80297219823148,
0.695309845677688));
#15564=CARTESIAN_POINT('Ctrl Pts',(-2.79611424068812,-3.81177525306492,
0.567000077065634));
#15565=CARTESIAN_POINT('Ctrl Pts',(-2.81626037388312,-3.82057831170534,
0.437238500388076));
#15566=CARTESIAN_POINT('Ctrl Pts',(-2.83008489722928,-3.82661907836333,
0.348194517165623));
#15567=CARTESIAN_POINT('Ctrl Pts',(-2.83948525764255,-3.83265984681399,
0.258467350941794));
#15568=CARTESIAN_POINT('Ctrl Pts',(-2.84454876096055,-3.83870060876577,
0.168492053738068));
#15569=CARTESIAN_POINT('Ctrl Pts',(-2.85240049093481,-3.84806772649144,
0.0289717071264769));
#15570=CARTESIAN_POINT('Ctrl Pts',(-2.84982609907032,-3.85743478090333,
-0.111064582497238));
#15571=CARTESIAN_POINT('Ctrl Pts',(-2.83719044067114,-3.86680180880028,
-0.250186399393045));
#15572=CARTESIAN_POINT('Ctrl Pts',(-2.82423457679865,-3.87640621044592,
-0.392833760096772));
#15573=CARTESIAN_POINT('Ctrl Pts',(-2.80070099369802,-3.88601058421576,
-0.534520981583524));
#15574=CARTESIAN_POINT('Ctrl Pts',(-2.76692914184924,-3.8956149697777,-0.673711919111808));
#15575=CARTESIAN_POINT('Ctrl Pts',(-2.74953893645332,-3.90056057472622,
-0.745385779452855));
#15576=CARTESIAN_POINT('Ctrl Pts',(-2.72943314510381,-3.90550618280147,
-0.81639771099666));
#15577=CARTESIAN_POINT('Ctrl Pts',(-2.70665285141107,-3.91045179941958,
-0.886536819547011));
#15578=CARTESIAN_POINT('Ctrl Pts',(-2.66722359737821,-3.91901191618605,
-1.00793704229967));
#15579=CARTESIAN_POINT('Ctrl Pts',(-2.61973805017892,-3.92757206551366,
-1.12684088972418));
#15580=CARTESIAN_POINT('Ctrl Pts',(-2.56442927732012,-3.93613223517365,
-1.24198315809337));
#15581=CARTESIAN_POINT('Ctrl Pts',(-2.51698367917274,-3.94347541689273,
-1.34075580323537));
#15582=CARTESIAN_POINT('Ctrl Pts',(-2.46378211843104,-3.95081861357388,
-1.43675993538346));
#15583=CARTESIAN_POINT('Ctrl Pts',(-2.40500101984259,-3.95816181749765,
-1.52920570699362));
#15584=CARTESIAN_POINT('Ctrl Pts',(-2.34085127496968,-3.96617569729187,
-1.63009481600624));
#15585=CARTESIAN_POINT('Ctrl Pts',(-2.27005625443048,-3.97418958571212,
-1.72674501095433));
#15586=CARTESIAN_POINT('Ctrl Pts',(-2.19345610618758,-3.98220347272476,
-1.81851953916284));
#15587=CARTESIAN_POINT('Ctrl Pts',(-2.10614697227237,-3.99133773095294,
-1.92312448781064));
#15588=CARTESIAN_POINT('Ctrl Pts',(-2.01131854196274,-4.00047190003977,
-2.02138198284188));
#15589=CARTESIAN_POINT('Ctrl Pts',(-1.91008620673602,-4.00960604015026,
-2.11252412289686));
#15590=CARTESIAN_POINT('Ctrl Pts',(-1.80722638330456,-4.01888702766141,
-2.20513153348582));
#15591=CARTESIAN_POINT('Ctrl Pts',(-1.6977541622283,-4.02816798525704,-2.29039382549714));
#15592=CARTESIAN_POINT('Ctrl Pts',(-1.58279871002626,-4.03744897605077,
-2.36747157972989));
#15593=CARTESIAN_POINT('Ctrl Pts',(-1.5146519473948,-4.04295084189958,-2.41316405730487));
#15594=CARTESIAN_POINT('Ctrl Pts',(-1.44457753941025,-4.04845271941498,
-2.45597958821667));
#15595=CARTESIAN_POINT('Ctrl Pts',(-1.37280618311532,-4.05395462174532,
-2.49573591232744));
#15596=CARTESIAN_POINT('Ctrl Pts',(-1.2646045336739,-4.0622492247449,-2.55567207720687));
#15597=CARTESIAN_POINT('Ctrl Pts',(-1.15246138914533,-4.07054384096858,
-2.60869580600677));
#15598=CARTESIAN_POINT('Ctrl Pts',(-1.03730936249408,-4.07883846677113,
-2.6540787781793));
#15599=CARTESIAN_POINT('Ctrl Pts',(-0.959063735452324,-4.08447465239349,
-2.68491643877395));
#15600=CARTESIAN_POINT('Ctrl Pts',(-0.879429643629576,-4.09011084243859,
-2.71222696854328));
#15601=CARTESIAN_POINT('Ctrl Pts',(-0.798706481232868,-4.09574703576282,
-2.73579384397682));
#15602=CARTESIAN_POINT('Ctrl Pts',(-0.680102865998873,-4.10402809022803,
-2.77041979944237));
#15603=CARTESIAN_POINT('Ctrl Pts',(-0.559148320148908,-4.11230915177202,
-2.79696178855869));
#15604=CARTESIAN_POINT('Ctrl Pts',(-0.437015001412886,-4.12059021676748,
-2.8155024676079));
#15605=CARTESIAN_POINT('Ctrl Pts',(-0.411863282802995,-4.12229559101516,
-2.81932067174014));
#15606=CARTESIAN_POINT('Ctrl Pts',(-0.386661587666493,-4.12400096540922,
-2.82279971732075));
#15607=CARTESIAN_POINT('Ctrl Pts',(-0.361420159933744,-4.12570633991797,
-2.82594059869468));
#15608=CARTESIAN_POINT('Ctrl Pts',(-0.227420491876474,-4.13475969539792,
-2.84261465794239));
#15609=CARTESIAN_POINT('Ctrl Pts',(-0.0922757684614264,-4.14381295104456,
-2.84976621078605));
#15610=CARTESIAN_POINT('Ctrl Pts',(0.0427129671981117,-4.15286617971873,
-2.8475412505536));
#15611=CARTESIAN_POINT('Ctrl Pts',(0.178702659926457,-4.16198653912936,
-2.84529979198401));
#15612=CARTESIAN_POINT('Ctrl Pts',(0.314535306910664,-4.17110687116603,
-2.83354221057195));
#15613=CARTESIAN_POINT('Ctrl Pts',(0.448884946130907,-4.18022725032238,
-2.8123658974596));
#15614=CARTESIAN_POINT('Ctrl Pts',(0.533489004344512,-4.18597063075535,
-2.7990305283607));
#15615=CARTESIAN_POINT('Ctrl Pts',(0.617504980397791,-4.19171402987412,
-2.78195903079779));
#15616=CARTESIAN_POINT('Ctrl Pts',(0.700599140013145,-4.19745746628173,
-2.76116539599247));
#15617=CARTESIAN_POINT('Ctrl Pts',(0.819351038141763,-4.20566555188416,
-2.73144870334458));
#15618=CARTESIAN_POINT('Ctrl Pts',(0.93627704500667,-4.21387363880933,-2.69410983378928));
#15619=CARTESIAN_POINT('Ctrl Pts',(1.05022883861694,-4.22208172614931,-2.64922295283315));
#15620=CARTESIAN_POINT('Ctrl Pts',(1.10229703136876,-4.22583226188203,-2.6287127116548));
#15621=CARTESIAN_POINT('Ctrl Pts',(1.15374432733471,-4.22958279770134,-2.60662725371738));
#15622=CARTESIAN_POINT('Ctrl Pts',(1.20446204849237,-4.23333333352066,-2.58297719187402));
#15623=CARTESIAN_POINT('Ctrl Pts',(1.31545832066639,-4.24154142105096,-2.53121877999393));
#15624=CARTESIAN_POINT('Ctrl Pts',(1.42295823404889,-4.24974950858126,-2.4719636913944));
#15625=CARTESIAN_POINT('Ctrl Pts',(1.52615212050412,-4.25795759520368,-2.40602519583505));
#15626=CARTESIAN_POINT('Ctrl Pts',(1.57330468230345,-4.26170813048258,-2.37589580451528));
#15627=CARTESIAN_POINT('Ctrl Pts',(1.61955860008734,-4.26545866557193,-2.34437162040238));
#15628=CARTESIAN_POINT('Ctrl Pts',(1.66483896157514,-4.2692092003851,-2.31153298290008));
#15629=CARTESIAN_POINT('Ctrl Pts',(1.77466818054188,-4.27830626356444,-2.23188163316914));
#15630=CARTESIAN_POINT('Ctrl Pts',(1.87883199843095,-4.2874032331951,-2.1444586779963));
#15631=CARTESIAN_POINT('Ctrl Pts',(1.97643042794329,-4.29650018319877,-2.05023587971271));
#15632=CARTESIAN_POINT('Ctrl Pts',(2.07391017921323,-4.3055860714462,-1.95612765495402));
#15633=CARTESIAN_POINT('Ctrl Pts',(2.16484137488291,-4.31467194011433,-1.85523520039081));
#15634=CARTESIAN_POINT('Ctrl Pts',(2.24829369710724,-4.32375786285549,-1.74848840006571));
#15635=CARTESIAN_POINT('Ctrl Pts',(2.30096046759489,-4.32949198977877,-1.68112048167632));
#15636=CARTESIAN_POINT('Ctrl Pts',(2.35064778296174,-4.33522613823866,-1.61142013221164));
#15637=CARTESIAN_POINT('Ctrl Pts',(2.39711249291075,-4.34096032674836,-1.53961569740268));
#15638=CARTESIAN_POINT('Ctrl Pts',(2.46421481110792,-4.3492413930114,-1.43591884794842));
#15639=CARTESIAN_POINT('Ctrl Pts',(2.52460350404338,-4.35752245657002,-1.32781167233767));
#15640=CARTESIAN_POINT('Ctrl Pts',(2.5774530717427,-4.36580351379685,-1.2161327212669));
#15641=CARTESIAN_POINT('Ctrl Pts',(2.58833673124962,-4.36750888644488,-1.19313393943277));
#15642=CARTESIAN_POINT('Ctrl Pts',(2.59890079988213,-4.36921425882437,-1.16998378268028));
#15643=CARTESIAN_POINT('Ctrl Pts',(2.60913830161044,-4.37091963090365,-1.14668972393339));
#15644=CARTESIAN_POINT('Ctrl Pts',(2.65893175317248,-4.37921426804059,-1.03339141965186));
#15645=CARTESIAN_POINT('Ctrl Pts',(2.70099558254949,-4.38750889807554,-0.916687593696909));
#15646=CARTESIAN_POINT('Ctrl Pts',(2.73525327248987,-4.39580351736332,-0.79775517172945));
#15647=CARTESIAN_POINT('Ctrl Pts',(2.75853132072395,-4.40143969855944,-0.716940771810146));
#15648=CARTESIAN_POINT('Ctrl Pts',(2.77820618530874,-4.40707587479338,-0.63509785969229));
#15649=CARTESIAN_POINT('Ctrl Pts',(2.79426743213858,-4.41271204492151,-0.552597573438769));
#15650=CARTESIAN_POINT('Ctrl Pts',(2.82068044144347,-4.42198082807486,-0.416924368764449));
#15651=CARTESIAN_POINT('Ctrl Pts',(2.83734960329111,-4.43124954080225,-0.279360307421618));
#15652=CARTESIAN_POINT('Ctrl Pts',(2.84422306735829,-4.44051824596736,-0.141307961682125));
#15653=CARTESIAN_POINT('Ctrl Pts',(2.8510260385497,-4.44969189314202,-0.00467145324992427));
#15654=CARTESIAN_POINT('Ctrl Pts',(2.84823318955168,-4.45886553290869,0.132444642262169));
#15655=CARTESIAN_POINT('Ctrl Pts',(2.83574436772078,-4.46803922621668,0.268682484355037));
#15656=CARTESIAN_POINT('Ctrl Pts',(2.82829134876046,-4.47351385873898,0.349985847793197));
#15657=CARTESIAN_POINT('Ctrl Pts',(2.81738424752888,-4.47898851032953,0.430976379224427));
#15658=CARTESIAN_POINT('Ctrl Pts',(2.80299319512765,-4.48446319394224,0.511363033623647));
#15659=CARTESIAN_POINT('Ctrl Pts',(2.78192745396434,-4.49247708095487,0.629033681144406));
#15660=CARTESIAN_POINT('Ctrl Pts',(2.7533952712281,-4.50049096937513,0.745391361015317));
#15661=CARTESIAN_POINT('Ctrl Pts',(2.71734439106664,-4.50850484916934,0.859383185828289));
#15662=CARTESIAN_POINT('Ctrl Pts',(2.67883587937714,-4.51706504471385,0.981145969390209));
#15663=CARTESIAN_POINT('Ctrl Pts',(2.63174833745007,-4.52562523041615,1.10020817320856));
#15664=CARTESIAN_POINT('Ctrl Pts',(2.57686399773131,-4.53418539404755,1.21555311043328));
#15665=CARTESIAN_POINT('Ctrl Pts',(2.52978249162659,-4.54152857059544,1.31449961127346));
#15666=CARTESIAN_POINT('Ctrl Pts',(2.4769646669258,-4.54887173090188,1.4107105849836));
#15667=CARTESIAN_POINT('Ctrl Pts',(2.41892952084411,-4.55621486724742,1.50356149313978));
#15668=CARTESIAN_POINT('Ctrl Pts',(2.34301936580719,-4.56581971286395,1.62501077533051));
#15669=CARTESIAN_POINT('Ctrl Pts',(2.25810592177126,-4.57542452625917,1.74085044412127));
#15670=CARTESIAN_POINT('Ctrl Pts',(2.16516849635887,-4.58502934710639,1.84985007122675));
#15671=CARTESIAN_POINT('Ctrl Pts',(2.07411849119096,-4.59443910839358,1.95663607877125));
#15672=CARTESIAN_POINT('Ctrl Pts',(1.97536620097115,-4.60384887683315,2.05685793011607));
#15673=CARTESIAN_POINT('Ctrl Pts',(1.86979798952804,-4.61325868973011,2.14932401144856));
#15674=CARTESIAN_POINT('Ctrl Pts',(1.81479773992408,-4.61816113196139,2.19749814913326));
#15675=CARTESIAN_POINT('Ctrl Pts',(1.75794693188286,-4.62306358625989,2.24356645717859));
#15676=CARTESIAN_POINT('Ctrl Pts',(1.699368297219,-4.62796605790107,2.28735537598812));
#15677=CARTESIAN_POINT('Ctrl Pts',(1.62718846358363,-4.63400681985281,2.34131151362912));
#15678=CARTESIAN_POINT('Ctrl Pts',(1.55241103130075,-4.64004758830341,2.39178593047225));
#15679=CARTESIAN_POINT('Ctrl Pts',(1.47531315044321,-4.64608835496136,2.43843210031673));
#15680=CARTESIAN_POINT('Ctrl Pts',(1.35950914751608,-4.65516182043095,2.5084964539556));
#15681=CARTESIAN_POINT('Ctrl Pts',(1.23846929110902,-4.66423528185609,2.56992132487734));
#15682=CARTESIAN_POINT('Ctrl Pts',(1.11366996284203,-4.67330871113862,2.62242170807228));
#15683=CARTESIAN_POINT('Ctrl Pts',(0.992589896059362,-4.68211173467034,
2.67335747825334));
#15684=CARTESIAN_POINT('Ctrl Pts',(0.867972296334286,-4.69091472794669,
2.71589279995554));
#15685=CARTESIAN_POINT('Ctrl Pts',(0.741175224670663,-4.69971766530755,
2.74981326359758));
#15686=CARTESIAN_POINT('Ctrl Pts',(0.594188688536139,-4.70992226430581,
2.78913476676327));
#15687=CARTESIAN_POINT('Ctrl Pts',(0.444077504545696,-4.72012688227234,
2.81694165833229));
#15688=CARTESIAN_POINT('Ctrl Pts',(0.292716472016533,-4.73033152301031,
2.83287479822956));
#15689=CARTESIAN_POINT('Ctrl Pts',(0.14629116648403,-4.74020340094969,2.8482883748851));
#15690=CARTESIAN_POINT('Ctrl Pts',(-0.00130505071413023,-4.75007530019963,
2.8525899300837));
#15691=CARTESIAN_POINT('Ctrl Pts',(-0.148370980131912,-4.75994722420332,
2.84540659185951));
#15692=CARTESIAN_POINT('Ctrl Pts',(-0.205585286096275,-4.76378778253413,
2.84261199685963));
#15693=CARTESIAN_POINT('Ctrl Pts',(-0.262719192545857,-4.76762834461144,
2.83807863098206));
#15694=CARTESIAN_POINT('Ctrl Pts',(-0.319671760795388,-4.77146891063799,
2.83178250052298));
#15695=CARTESIAN_POINT('Ctrl Pts',(-0.37998387149061,-4.77553602561533,
2.82511497122851));
#15696=CARTESIAN_POINT('Ctrl Pts',(-0.440068487676707,-4.77960314668888,
2.81647300524789));
#15697=CARTESIAN_POINT('Ctrl Pts',(-0.499795169357878,-4.78367027013473,
2.8058340629029));
#15698=CARTESIAN_POINT('Ctrl Pts',(-0.646934880785383,-4.79368983514851,
2.77962448851381));
#15699=CARTESIAN_POINT('Ctrl Pts',(-0.791900799561659,-4.80370941455995,
2.74129173439158));
#15700=CARTESIAN_POINT('Ctrl Pts',(-0.932987708459681,-4.81372895269081,
2.69185259721203));
#15701=CARTESIAN_POINT('Ctrl Pts',(-1.07141349208279,-4.82355950627043,
2.6433459614144));
#15702=CARTESIAN_POINT('Ctrl Pts',(-1.20610416138044,-4.833390020112,2.584148780273));
#15703=CARTESIAN_POINT('Ctrl Pts',(-1.33547704634397,-4.84322044162881,
2.51526142986738));
#15704=CARTESIAN_POINT('Ctrl Pts',(-1.48479827299402,-4.85456664141242,
2.43575215969737));
#15705=CARTESIAN_POINT('Ctrl Pts',(-1.62728010749542,-4.86591292611561,
2.34321424573768));
#15706=CARTESIAN_POINT('Ctrl Pts',(-1.7606072822343,-4.87725924518256,2.23897728299655));
#15707=CARTESIAN_POINT('Ctrl Pts',(-1.88728409303887,-4.88803960947504,
2.13993966344253));
#15708=CARTESIAN_POINT('Ctrl Pts',(-2.00569749096051,-4.89882000478868,
2.03034012677808));
#15709=CARTESIAN_POINT('Ctrl Pts',(-2.11382090529319,-4.90960038776174,
1.91129521590937));
#15710=CARTESIAN_POINT('Ctrl Pts',(-2.13177852458187,-4.91139084188688,
1.89152370572511));
#15711=CARTESIAN_POINT('Ctrl Pts',(-2.14945219484852,-4.91318129567162,
1.87149161408109));
#15712=CARTESIAN_POINT('Ctrl Pts',(-2.16683249404356,-4.9149717489173,1.85120401255983));
#15713=CARTESIAN_POINT('Ctrl Pts',(-2.18715210290924,-4.91706499882263,
1.82748542618174));
#15714=CARTESIAN_POINT('Ctrl Pts',(-2.20706535664628,-4.9191582509282,1.80342384886703));
#15715=CARTESIAN_POINT('Ctrl Pts',(-2.22655731073033,-4.9212515046306,1.77902853884047));
#15716=CARTESIAN_POINT('Ctrl Pts',(-2.33801743056546,-4.93322127982647,
1.63952974014388));
#15717=CARTESIAN_POINT('Ctrl Pts',(-2.43569777707777,-4.94519110723601,
1.48911776930381));
#15718=CARTESIAN_POINT('Ctrl Pts',(-2.5186153379613,-4.95716087402997,1.33095551518211));
#15719=CARTESIAN_POINT('Ctrl Pts',(-2.58687764345666,-4.96701504567819,
1.20074763166928));
#15720=CARTESIAN_POINT('Ctrl Pts',(-2.64513519268278,-4.97686917624427,
1.0652876964692));
#15721=CARTESIAN_POINT('Ctrl Pts',(-2.69286608630087,-4.98672320277401,
0.926338234405749));
#15722=CARTESIAN_POINT('Ctrl Pts',(-2.75720448791769,-5.00000584360378,
0.739042635747796));
#15723=CARTESIAN_POINT('Ctrl Pts',(-2.80254615611727,-5.01328865684996,
0.545045070540891));
#15724=CARTESIAN_POINT('Ctrl Pts',(-2.82744790125318,-5.02657150224111,
0.348481808485192));
#15725=CARTESIAN_POINT('Ctrl Pts',(-2.84738445471526,-5.03720586364123,
0.191111553458274));
#15726=CARTESIAN_POINT('Ctrl Pts',(-2.85421898098582,-5.04784024564545,
0.0320971413027112));
#15727=CARTESIAN_POINT('Ctrl Pts',(-2.84719447964139,-5.05847457627068,
-0.126420910195643));
#15728=CARTESIAN_POINT('Ctrl Pts',(-2.84711547783896,-5.05859417640254,
-0.128203700342931));
#15729=CARTESIAN_POINT('Ctrl Pts',(-2.8470347242005,-5.05871377654117,-0.129986398137237));
#15730=CARTESIAN_POINT('Ctrl Pts',(-2.84695221781174,-5.05883337668647,
-0.131769000519424));
#15731=CARTESIAN_POINT('Ctrl Pts',(-2.83756453871079,-5.07244162934965,
-0.334595707407065));
#15732=CARTESIAN_POINT('Ctrl Pts',(-2.80548826042884,-5.08604996832765,
-0.536183502277633));
#15733=CARTESIAN_POINT('Ctrl Pts',(-2.75271150410846,-5.09965823826323,
-0.732204056437572));
#15734=CARTESIAN_POINT('Ctrl Pts',(-2.71319448789317,-5.10984753865225,
-0.878976006010336));
#15735=CARTESIAN_POINT('Ctrl Pts',(-2.66207125303721,-5.12003680033345,
-1.02262775397972));
#15736=CARTESIAN_POINT('Ctrl Pts',(-2.60016461395293,-5.1302259580906,-1.16135726039429));
#15737=CARTESIAN_POINT('Ctrl Pts',(-2.52524568289888,-5.14255679721866,
-1.32924662541192));
#15738=CARTESIAN_POINT('Ctrl Pts',(-2.43439483816887,-5.15488779965095,
-1.49022775634066));
#15739=CARTESIAN_POINT('Ctrl Pts',(-2.32895182834645,-5.16721884125924,
-1.64096625492276));
#15740=CARTESIAN_POINT('Ctrl Pts',(-2.24573172623983,-5.17695102306484,
-1.75993548071144));
#15741=CARTESIAN_POINT('Ctrl Pts',(-2.15342339325781,-5.18668322927331,
-1.87252384289964));
#15742=CARTESIAN_POINT('Ctrl Pts',(-2.05270819500149,-5.19641539886041,
-1.9770910616754));
#15743=CARTESIAN_POINT('Ctrl Pts',(-2.0335216961287,-5.19826940167276,-1.99701138015669));
#15744=CARTESIAN_POINT('Ctrl Pts',(-2.01403015453902,-5.20012340315607,
-2.01664061147923));
#15745=CARTESIAN_POINT('Ctrl Pts',(-1.99424446419597,-5.20197740288845,
-2.03597332011536));
#15746=CARTESIAN_POINT('Ctrl Pts',(-1.87755085247301,-5.21291206936477,
-2.14999530044671));
#15747=CARTESIAN_POINT('Ctrl Pts',(-1.75079332881031,-5.22384676134255,
-2.25354437627423));
#15748=CARTESIAN_POINT('Ctrl Pts',(-1.61619727332964,-5.23478142843354,
-2.34565521913265));
#15749=CARTESIAN_POINT('Ctrl Pts',(-1.4742672465223,-5.24631191190731,-2.44278506702792));
#15750=CARTESIAN_POINT('Ctrl Pts',(-1.32362032921175,-5.25784236770832,
-2.52719705812083));
#15751=CARTESIAN_POINT('Ctrl Pts',(-1.16681718870844,-5.26937273675464,
-2.59773035429892));
#15752=CARTESIAN_POINT('Ctrl Pts',(-1.14707129845689,-5.27082473191888,
-2.60661246419125));
#15753=CARTESIAN_POINT('Ctrl Pts',(-1.12722773442568,-5.27227672570737,
-2.61527444208103));
#15754=CARTESIAN_POINT('Ctrl Pts',(-1.10729157078743,-5.27372871800215,
-2.62371392855201));
#15755=CARTESIAN_POINT('Ctrl Pts',(-0.967477248542152,-5.2839116861139,
-2.68290089663921));
#15756=CARTESIAN_POINT('Ctrl Pts',(-0.822904805739579,-5.29409475555286,
-2.73122652109907));
#15757=CARTESIAN_POINT('Ctrl Pts',(-0.675423581781764,-5.30427786596671,
-2.76774962167252));
#15758=CARTESIAN_POINT('Ctrl Pts',(-0.531952285489216,-5.31418410360266,
-2.80327968064053));
#15759=CARTESIAN_POINT('Ctrl Pts',(-0.385729529005817,-5.3240903800156,
-2.82763991308817));
#15760=CARTESIAN_POINT('Ctrl Pts',(-0.238481853495246,-5.33399663964339,
-2.84000464883967));
#15761=CARTESIAN_POINT('Ctrl Pts',(-0.181583991961912,-5.33782450984006,
-2.84478249691263));
#15762=CARTESIAN_POINT('Ctrl Pts',(-0.124533255816757,-5.34165237753051,
-2.84776974350696));
#15763=CARTESIAN_POINT('Ctrl Pts',(-0.0674358860842899,-5.34548023950904,
-2.84899499112165));
#15764=CARTESIAN_POINT('Ctrl Pts',(0.0804325551778038,-5.3553934804654,
-2.85216808746204));
#15765=CARTESIAN_POINT('Ctrl Pts',(0.228462621505615,-5.36530670065781,
-2.84352538719917));
#15766=CARTESIAN_POINT('Ctrl Pts',(0.374965744204218,-5.37521989870767,
-2.82362224019619));
#15767=CARTESIAN_POINT('Ctrl Pts',(0.527029781898301,-5.38550937850958,
-2.80296361640482));
#15768=CARTESIAN_POINT('Ctrl Pts',(0.677450029835101,-5.39579883445611,
-2.77017343020061));
#15769=CARTESIAN_POINT('Ctrl Pts',(0.824346177097707,-5.40608826500567,
-2.7258178741885));
#15770=CARTESIAN_POINT('Ctrl Pts',(0.877374657186616,-5.40980267735202,
-2.70980582919854));
#15771=CARTESIAN_POINT('Ctrl Pts',(0.929943866829867,-5.41351708638873,
-2.69228613387777));
#15772=CARTESIAN_POINT('Ctrl Pts',(0.98196507546841,-5.4172314920433,-2.67328379028232));
#15773=CARTESIAN_POINT('Ctrl Pts',(1.11023950482274,-5.42639051157012,-2.62642761671593));
#15774=CARTESIAN_POINT('Ctrl Pts',(1.23533711721485,-5.43554959431835,-2.57049493875236));
#15775=CARTESIAN_POINT('Ctrl Pts',(1.35576092762186,-5.44470870962387,-2.50586711172746));
#15776=CARTESIAN_POINT('Ctrl Pts',(1.47352135254951,-5.45366525490087,-2.44266864336079));
#15777=CARTESIAN_POINT('Ctrl Pts',(1.58681131404656,-5.46262183131094,-2.37115588388267));
#15778=CARTESIAN_POINT('Ctrl Pts',(1.69424514700893,-5.4715784101799,-2.29173152475888));
#15779=CARTESIAN_POINT('Ctrl Pts',(1.76383466535031,-5.47737997186946,-2.24028494835374));
#15780=CARTESIAN_POINT('Ctrl Pts',(1.83096748386614,-5.48318153459071,-2.18551985140271));
#15781=CARTESIAN_POINT('Ctrl Pts',(1.89542786570679,-5.48898309055072,-2.1277636357077));
#15782=CARTESIAN_POINT('Ctrl Pts',(1.99996535344416,-5.49839166164059,-2.03409851121464));
#15783=CARTESIAN_POINT('Ctrl Pts',(2.09741321270494,-5.50780017341223,-1.93262981881011));
#15784=CARTESIAN_POINT('Ctrl Pts',(2.18701354397179,-5.51720865915534,-1.82464990341988));
#15785=CARTESIAN_POINT('Ctrl Pts',(2.27899284570153,-5.52686694877045,-1.71380302285589));
#15786=CARTESIAN_POINT('Ctrl Pts',(2.36270322802092,-5.53652521095654,-1.59609363458982));
#15787=CARTESIAN_POINT('Ctrl Pts',(2.43729095147334,-5.54618348172593,-1.47287733500589));
#15788=CARTESIAN_POINT('Ctrl Pts',(2.47474798900839,-5.55103374654147,-1.41099962450852));
#15789=CARTESIAN_POINT('Ctrl Pts',(2.50990375352354,-5.55588401352164,-1.34773254351142));
#15790=CARTESIAN_POINT('Ctrl Pts',(2.54264596413126,-5.56073428722735,-1.28324507982158));
#15791=CARTESIAN_POINT('Ctrl Pts',(2.60074923441848,-5.56934142641736,-1.16880770789828));
#15792=CARTESIAN_POINT('Ctrl Pts',(2.65130641309992,-5.5779486010165,-1.05040875527548));
#15793=CARTESIAN_POINT('Ctrl Pts',(2.69358203153906,-5.58655579730455,-0.929126797966435));
#15794=CARTESIAN_POINT('Ctrl Pts',(2.73059279732476,-5.59409108449017,-0.822948857069878));
#15795=CARTESIAN_POINT('Ctrl Pts',(2.76125653093975,-5.60162638829895,-0.714562292579616));
#15796=CARTESIAN_POINT('Ctrl Pts',(2.78510865337264,-5.6091616995248,-0.604706365635819));
#15797=CARTESIAN_POINT('Ctrl Pts',(2.8097186803481,-5.6169364463239,-0.49135975117377));
#15798=CARTESIAN_POINT('Ctrl Pts',(2.82707707960445,-5.62471120101895,-0.376449536131305));
#15799=CARTESIAN_POINT('Ctrl Pts',(2.83731951212943,-5.63248595349808,-0.26092697658365));
#15800=CARTESIAN_POINT('Ctrl Pts',(2.84937910293163,-5.64164006149519,-0.12490901472063));
#15801=CARTESIAN_POINT('Ctrl Pts',(2.85157945535316,-5.65079408277546,0.0119261659157435));
#15802=CARTESIAN_POINT('Ctrl Pts',(2.84417579217258,-5.65994807517877,0.148238094356482));
#15803=CARTESIAN_POINT('Ctrl Pts',(2.83664510333784,-5.6692591238723,0.286888745056287));
#15804=CARTESIAN_POINT('Ctrl Pts',(2.81917796946369,-5.6785701426895,0.424999299784865));
#15805=CARTESIAN_POINT('Ctrl Pts',(2.79198999722367,-5.68788119249867,0.561164284972185));
#15806=CARTESIAN_POINT('Ctrl Pts',(2.77607045508886,-5.69333314928484,0.640893813891735));
#15807=CARTESIAN_POINT('Ctrl Pts',(2.75681711012934,-5.69878511669668,0.71995629975189));
#15808=CARTESIAN_POINT('Ctrl Pts',(2.73426515074854,-5.70423710695368,0.798067696028705));
#15809=CARTESIAN_POINT('Ctrl Pts',(2.69986398426108,-5.71255367144159,0.917220231846649));
#15810=CARTESIAN_POINT('Ctrl Pts',(2.65775494410319,-5.7208702511505,1.03425194984188));
#15811=CARTESIAN_POINT('Ctrl Pts',(2.60808881511018,-5.7291868416733,1.14798084834381));
#15812=CARTESIAN_POINT('Ctrl Pts',(2.5731333343602,-5.73504013497034,1.22802429853621));
#15813=CARTESIAN_POINT('Ctrl Pts',(2.53443556790553,-5.74089343362401,1.30643163648447));
#15814=CARTESIAN_POINT('Ctrl Pts',(2.49206304447104,-5.74674673609787,1.38279491692253));
#15815=CARTESIAN_POINT('Ctrl Pts',(2.43196952830668,-5.75504800065133,1.49109476917145));
#15816=CARTESIAN_POINT('Ctrl Pts',(2.36448332309234,-5.76334927288853,1.59528160281069));
#15817=CARTESIAN_POINT('Ctrl Pts',(2.29050189237751,-5.7716505484267,1.69458502869615));
#15818=CARTESIAN_POINT('Ctrl Pts',(2.27761425207795,-5.77309663904876,1.7118837862487));
#15819=CARTESIAN_POINT('Ctrl Pts',(2.26452960469196,-5.77454272977099,1.72903443523847));
#15820=CARTESIAN_POINT('Ctrl Pts',(2.25125281022662,-5.77598882057022,1.74603301441406));
#15821=CARTESIAN_POINT('Ctrl Pts',(2.16812732437095,-5.78504273795906,1.85246044736981));
#15822=CARTESIAN_POINT('Ctrl Pts',(2.07746093396082,-5.79409655590333,1.9529454960784));
#15823=CARTESIAN_POINT('Ctrl Pts',(1.98028264461572,-5.80315034641737,2.04667701103836));
#15824=CARTESIAN_POINT('Ctrl Pts',(1.88228616404374,-5.81228036519205,2.14119769715721));
#15825=CARTESIAN_POINT('Ctrl Pts',(1.77766674968735,-5.82141035607266,2.22885151585887));
#15826=CARTESIAN_POINT('Ctrl Pts',(1.66743971161223,-5.83054039290774,2.30877304976365));
#15827=CARTESIAN_POINT('Ctrl Pts',(1.59822319673337,-5.83627355367733,2.35895937552604));
#15828=CARTESIAN_POINT('Ctrl Pts',(1.5267947663949,-5.84200673256746,2.40609603228708));
#15829=CARTESIAN_POINT('Ctrl Pts',(1.45340037684324,-5.84773994786366,2.44995969872409));
#15830=CARTESIAN_POINT('Ctrl Pts',(1.34833164615637,-5.8559474097365,2.51275332346791));
#15831=CARTESIAN_POINT('Ctrl Pts',(1.23917579451082,-5.86415487372048,2.56886748694508));
#15832=CARTESIAN_POINT('Ctrl Pts',(1.12680042373391,-5.87236233910441,2.61754633616288));
#15833=CARTESIAN_POINT('Ctrl Pts',(1.07216724228544,-5.87635253680033,2.64121237956396));
#15834=CARTESIAN_POINT('Ctrl Pts',(1.01677359388372,-5.88034273482714,2.66312162629128));
#15835=CARTESIAN_POINT('Ctrl Pts',(0.960721486505664,-5.88433293310313,
2.68319105271398));
#15836=CARTESIAN_POINT('Ctrl Pts',(0.845451670024785,-5.8925386803,2.72446334752742));
#15837=CARTESIAN_POINT('Ctrl Pts',(0.727396622634277,-5.90074442855068,
2.75795152729709));
#15838=CARTESIAN_POINT('Ctrl Pts',(0.607702879355788,-5.90895017714448,
2.78366462868508));
#15839=CARTESIAN_POINT('Ctrl Pts',(0.556448060882608,-5.91246401289806,
2.79467539923937));
#15840=CARTESIAN_POINT('Ctrl Pts',(0.504892884501329,-5.91597784871455,
2.8042611070848));
#15841=CARTESIAN_POINT('Ctrl Pts',(0.453127606679704,-5.91949168453815,
2.81242536210152));
#15842=CARTESIAN_POINT('Ctrl Pts',(0.319234225988536,-5.92858038989074,
2.83354260035493));
#15843=CARTESIAN_POINT('Ctrl Pts',(0.183869595833746,-5.93766899938026,
2.8451657633036));
#15844=CARTESIAN_POINT('Ctrl Pts',(0.0483532896092884,-5.94675758765968,
2.8473542009551));
#15845=CARTESIAN_POINT('Ctrl Pts',(-0.0871603316276508,-5.9558459958667,
2.84954259524703));
#15846=CARTESIAN_POINT('Ctrl Pts',(-0.222826888457978,-5.96493438286443,
2.84229661416303));
#15847=CARTESIAN_POINT('Ctrl Pts',(-0.357330541496659,-5.97402282330132,
2.82562460597089));
#15848=CARTESIAN_POINT('Ctrl Pts',(-0.442278735615453,-5.97976279084144,
2.81509510021948));
#15849=CARTESIAN_POINT('Ctrl Pts',(-0.526763083009378,-5.98550277969727,
2.8008047422449));
#15850=CARTESIAN_POINT('Ctrl Pts',(-0.610449379425582,-5.99124280867417,
2.78274520582773));
#15851=CARTESIAN_POINT('Ctrl Pts',(-0.731085633271099,-5.99951722900809,
2.7567118537396));
#15852=CARTESIAN_POINT('Ctrl Pts',(-0.850088999337008,-6.00779164691864,
2.72283472405422));
#15853=CARTESIAN_POINT('Ctrl Pts',(-0.966285437540862,-6.01606605918477,
2.68112815680615));
#15854=CARTESIAN_POINT('Ctrl Pts',(-0.993684309326853,-6.01801714791252,
2.671293837387));
#15855=CARTESIAN_POINT('Ctrl Pts',(-1.0209271484257,-6.01996823632644,2.66102442127421));
#15856=CARTESIAN_POINT('Ctrl Pts',(-1.04799865446575,-6.0219193243843,2.6503205127232));
#15857=CARTESIAN_POINT('Ctrl Pts',(-1.16296636172232,-6.03020523652882,
2.60486298173203));
#15858=CARTESIAN_POINT('Ctrl Pts',(-1.27484199587427,-6.03849114225165,
2.5515654815248));
#15859=CARTESIAN_POINT('Ctrl Pts',(-1.38274512718447,-6.04677703831838,
2.4912081959808));
#15860=CARTESIAN_POINT('Ctrl Pts',(-1.45314261769349,-6.05218287114856,
2.4518302707562));
#15861=CARTESIAN_POINT('Ctrl Pts',(-1.52184967133763,-6.05758869986867,
2.40944842689175));
#15862=CARTESIAN_POINT('Ctrl Pts',(-1.58862902491494,-6.06299452358051,
2.36428881032277));
#15863=CARTESIAN_POINT('Ctrl Pts',(-1.70302589983738,-6.07225501063062,
2.28692778881772));
#15864=CARTESIAN_POINT('Ctrl Pts',(-1.81186251619505,-6.08151542614159,
2.20135783068163));
#15865=CARTESIAN_POINT('Ctrl Pts',(-1.9141178692562,-6.09077583323541,2.10853699469762));
#15866=CARTESIAN_POINT('Ctrl Pts',(-2.01540941019701,-6.09994895597365,
2.01659104539743));
#15867=CARTESIAN_POINT('Ctrl Pts',(-2.11024405254985,-6.10912207045263,
1.91752935253497));
#15868=CARTESIAN_POINT('Ctrl Pts',(-2.19759562695022,-6.11829523802621,
1.81224624033903));
#15869=CARTESIAN_POINT('Ctrl Pts',(-2.24981189452375,-6.12377869468749,
1.74931101341112));
#15870=CARTESIAN_POINT('Ctrl Pts',(-2.29935352499215,-6.12926217032111,
1.68415204005637));
#15871=CARTESIAN_POINT('Ctrl Pts',(-2.34599349219481,-6.13474567803236,
1.6169559696464));
#15872=CARTESIAN_POINT('Ctrl Pts',(-2.41618993206687,-6.14299874385612,
1.51582114475093));
#15873=CARTESIAN_POINT('Ctrl Pts',(-2.47980005198525,-6.15125181256872,
1.41008201180028));
#15874=CARTESIAN_POINT('Ctrl Pts',(-2.5359725440974,-6.1595048717156,1.30051653404565));
#15875=CARTESIAN_POINT('Ctrl Pts',(-2.59396801765886,-6.16802576967752,
1.18739529748593));
#15876=CARTESIAN_POINT('Ctrl Pts',(-2.64403449050075,-6.17654665744279,
1.07019614130459));
#15877=CARTESIAN_POINT('Ctrl Pts',(-2.68601873281737,-6.18506752130453,
0.950178909542243));
#15878=CARTESIAN_POINT('Ctrl Pts',(-2.72121537483224,-6.19221081551329,
0.849564886068879));
#15879=CARTESIAN_POINT('Ctrl Pts',(-2.75073267587082,-6.19935409292271,
0.746971150019362));
#15880=CARTESIAN_POINT('Ctrl Pts',(-2.7745081152172,-6.20649734545702,0.643144978464038));
#15881=CARTESIAN_POINT('Ctrl Pts',(-2.80583618147833,-6.21590975990097,
0.506336857497832));
#15882=CARTESIAN_POINT('Ctrl Pts',(-2.82723626244033,-6.22532213968569,
0.367244546698496));
#15883=CARTESIAN_POINT('Ctrl Pts',(-2.83855637370735,-6.23473452843586,
0.227335517427473));
#15884=CARTESIAN_POINT('Ctrl Pts',(-2.8496594598203,-6.24396646621073,0.0901087743916822));
#15885=CARTESIAN_POINT('Ctrl Pts',(-2.8510653530964,-6.25319841261058,-0.0479049212921638));
#15886=CARTESIAN_POINT('Ctrl Pts',(-2.84258167957677,-6.26243040879888,
-0.185321199119131));
#15887=CARTESIAN_POINT('Ctrl Pts',(-2.83773638421417,-6.267703095002,-0.26380399930707));
#15888=CARTESIAN_POINT('Ctrl Pts',(-2.82966429723861,-6.2729757974457,-0.342091832328108));
#15889=CARTESIAN_POINT('Ctrl Pts',(-2.81832220863144,-6.27824852379865,
-0.419924497124111));
#15890=CARTESIAN_POINT('Ctrl Pts',(-2.80481332035976,-6.28452855507472,
-0.512626362629817));
#15891=CARTESIAN_POINT('Ctrl Pts',(-2.78666789891511,-6.2908085874816,-0.604654818892115));
#15892=CARTESIAN_POINT('Ctrl Pts',(-2.76383203365409,-6.29708861758833,
-0.695508798970515));
#15893=CARTESIAN_POINT('Ctrl Pts',(-2.73172566074844,-6.30591810515803,
-0.823246098653206));
#15894=CARTESIAN_POINT('Ctrl Pts',(-2.69034550062392,-6.31474758818097,
-0.948660552264399));
#15895=CARTESIAN_POINT('Ctrl Pts',(-2.64045788613141,-6.32357705712189,
-1.07060594415041));
#15896=CARTESIAN_POINT('Ctrl Pts',(-2.5906928614993,-6.33238482922731,-1.19225167711871));
#15897=CARTESIAN_POINT('Ctrl Pts',(-2.53246286639955,-6.34119258731979,
-1.31044437710593));
#15898=CARTESIAN_POINT('Ctrl Pts',(-2.46657308311698,-6.35000032193402,
-1.42407257589893));
#15899=CARTESIAN_POINT('',(-1.86074722859424,-6.34999975408592,-1.07430190765501));
#15900=CARTESIAN_POINT('Ctrl Pts',(-1.86074679171387,-6.34999975408563,
-1.07430266108979));
#15901=CARTESIAN_POINT('Ctrl Pts',(-1.8607430428313,-6.37442981441701,-1.07430049667143));
#15902=CARTESIAN_POINT('Ctrl Pts',(-1.86369055307458,-6.398701888929,-1.07600224250384));
#15903=CARTESIAN_POINT('Ctrl Pts',(-1.87454995456356,-6.4464134230453,-1.08227192087675));
#15904=CARTESIAN_POINT('Ctrl Pts',(-1.88253671298855,-6.46974575644526,
-1.08688307800337));
#15905=CARTESIAN_POINT('Ctrl Pts',(-1.91354213791911,-6.53898582858574,
-1.10478406843336));
#15906=CARTESIAN_POINT('Ctrl Pts',(-1.94373429399608,-6.58153621615069,
-1.12221551787182));
#15907=CARTESIAN_POINT('Ctrl Pts',(-2.00822303235105,-6.64385578994547,
-1.15944810832076));
#15908=CARTESIAN_POINT('Ctrl Pts',(-2.04167479775446,-6.66700783322522,
-1.17876149408129));
#15909=CARTESIAN_POINT('Ctrl Pts',(-2.10551567089605,-6.69360737099446,
-1.21562003937489));
#15910=CARTESIAN_POINT('Ctrl Pts',(-2.13510937709143,-6.70025495629181,
-1.23270597361311));
#15911=CARTESIAN_POINT('Ctrl Pts',(-2.19496906237396,-6.69982796752831,
-1.26726597902458));
#15912=CARTESIAN_POINT('Ctrl Pts',(-2.22452519635254,-6.69282040482862,
-1.28433022093333));
#15913=CARTESIAN_POINT('Ctrl Pts',(-2.288485768463,-6.66533843223848,-1.32125787445883));
#15914=CARTESIAN_POINT('Ctrl Pts',(-2.32200562531788,-6.64162093032346,
-1.34061057283719));
#15915=CARTESIAN_POINT('Ctrl Pts',(-2.38620384795508,-6.57824524282073,
-1.37767543395828));
#15916=CARTESIAN_POINT('Ctrl Pts',(-2.41606512644336,-6.53526148665362,
-1.39491585113183));
#15917=CARTESIAN_POINT('Ctrl Pts',(-2.44604492211185,-6.46620259780363,
-1.41222469423128));
#15918=CARTESIAN_POINT('Ctrl Pts',(-2.45357470056292,-6.44352512622915,
-1.41657201384694));
#15919=CARTESIAN_POINT('Ctrl Pts',(-2.46380600196008,-6.39721118892435,
-1.42247905846275));
#15920=CARTESIAN_POINT('Ctrl Pts',(-2.46657490953438,-6.37367868071213,
-1.42407768799611));
#15921=CARTESIAN_POINT('Ctrl Pts',(-2.46657132033207,-6.35000032196148,
-1.42407561576919));
#15922=CARTESIAN_POINT('Ctrl Pts',(2.01902767720344,-2.11666691256093,0.73486875714661));
#15923=CARTESIAN_POINT('Ctrl Pts',(1.98328697402221,-2.126004011307,0.833645723886708));
#15924=CARTESIAN_POINT('Ctrl Pts',(1.94040529944881,-2.13534109246068,0.929939958542491));
#15925=CARTESIAN_POINT('Ctrl Pts',(1.89068523013276,-2.1446781618249,1.02255013903026));
#15926=CARTESIAN_POINT('Ctrl Pts',(1.84649040156668,-2.15297763094347,1.10486883058545));
#15927=CARTESIAN_POINT('Ctrl Pts',(1.79689349372479,-2.16127709074722,1.18427617526517));
#15928=CARTESIAN_POINT('Ctrl Pts',(1.74213944561929,-2.16957654531166,1.25994053526106));
#15929=CARTESIAN_POINT('Ctrl Pts',(1.6892295996948,-2.17759646123489,1.33305640098927));
#15930=CARTESIAN_POINT('Ctrl Pts',(1.63150474578687,-2.18561637226582,1.40267685173721));
#15931=CARTESIAN_POINT('Ctrl Pts',(1.56962782965123,-2.1936362820818,1.46836171795241));
#15932=CARTESIAN_POINT('Ctrl Pts',(1.49433665037739,-2.20339482380342,1.54828637074126));
#15933=CARTESIAN_POINT('Ctrl Pts',(1.4129141324678,-2.2131534514039,1.62237850708974));
#15934=CARTESIAN_POINT('Ctrl Pts',(1.32642445619322,-2.22291210493305,1.68999096418341));
#15935=CARTESIAN_POINT('Ctrl Pts',(1.23875871499644,-2.23280345418495,1.75852279850818));
#15936=CARTESIAN_POINT('Ctrl Pts',(1.1458860079854,-2.24269483007546,1.82039837823104));
#15937=CARTESIAN_POINT('Ctrl Pts',(1.04887678686688,-2.25258617017529,1.87490705154322));
#15938=CARTESIAN_POINT('Ctrl Pts',(0.989966237882138,-2.25859285973281,
1.90800839832475));
#15939=CARTESIAN_POINT('Ctrl Pts',(0.929529589478074,-2.26459953609166,
1.93839225646822));
#15940=CARTESIAN_POINT('Ctrl Pts',(0.867802501469699,-2.27060618527117,
1.96589098130968));
#15941=CARTESIAN_POINT('Ctrl Pts',(0.776313466021059,-2.27950896292428,
2.0066483196677));
#15942=CARTESIAN_POINT('Ctrl Pts',(0.681931515948534,-2.28841172914792,
2.04108740306593));
#15943=CARTESIAN_POINT('Ctrl Pts',(0.585569263820482,-2.29731449308824,
2.06858465183689));
#15944=CARTESIAN_POINT('Ctrl Pts',(0.550019481933898,-2.30059888411561,
2.07872888544187));
#15945=CARTESIAN_POINT('Ctrl Pts',(0.514200436844675,-2.30388327483221,
2.08792876916703));
#15946=CARTESIAN_POINT('Ctrl Pts',(0.478158691722409,-2.30716766569729,
2.09615463779207));
#15947=CARTESIAN_POINT('Ctrl Pts',(0.380459348914482,-2.31607075371241,
2.11845272452356));
#15948=CARTESIAN_POINT('Ctrl Pts',(0.281123326237266,-2.32497384281853,
2.13358987550845));
#15949=CARTESIAN_POINT('Ctrl Pts',(0.181242420447869,-2.33387694216285,
2.14170712218003));
#15950=CARTESIAN_POINT('Ctrl Pts',(0.130015470738463,-2.33844316649537,
2.14587029815183));
#15951=CARTESIAN_POINT('Ctrl Pts',(0.078645281922746,-2.34300939352099,
2.14818777343025));
#15952=CARTESIAN_POINT('Ctrl Pts',(0.0272788198494572,-2.34757562447378,
2.14868386556989));
#15953=CARTESIAN_POINT('Ctrl Pts',(-0.0870156521548496,-2.35773585227095,
2.14978771011898));
#15954=CARTESIAN_POINT('Ctrl Pts',(-0.201396983616965,-2.3678961366145,
2.14188078703598));
#15955=CARTESIAN_POINT('Ctrl Pts',(-0.314478908535946,-2.37805642767878,
2.12517596726398));
#15956=CARTESIAN_POINT('Ctrl Pts',(-0.426117761075774,-2.38808706021975,
2.10868432271012));
#15957=CARTESIAN_POINT('Ctrl Pts',(-0.536491503978643,-2.398117699311,2.08361760213658));
#15958=CARTESIAN_POINT('Ctrl Pts',(-0.64425804797752,-2.4081482970102,2.05013182659052));
#15959=CARTESIAN_POINT('Ctrl Pts',(-0.702980846087058,-2.41361404492927,
2.03188517634113));
#15960=CARTESIAN_POINT('Ctrl Pts',(-0.760929242478707,-2.41907978055806,
2.01113787810776));
#15961=CARTESIAN_POINT('Ctrl Pts',(-0.817882895186075,-2.42454549613965,
1.98790940623174));
#15962=CARTESIAN_POINT('Ctrl Pts',(-0.888083410572842,-2.4312824837172,
1.95927821894472));
#15963=CARTESIAN_POINT('Ctrl Pts',(-0.956747742671155,-2.43801946488298,
1.92688588256022));
#15964=CARTESIAN_POINT('Ctrl Pts',(-1.02341716322646,-2.44475644852306,
1.89079806175955));
#15965=CARTESIAN_POINT('Ctrl Pts',(-1.12079483922406,-2.45459651919776,
1.83808801730262));
#15966=CARTESIAN_POINT('Ctrl Pts',(-1.2139148019473,-2.46443659515107,1.77749245331374));
#15967=CARTESIAN_POINT('Ctrl Pts',(-1.3018249097566,-2.47427670407209,1.71009504716673));
#15968=CARTESIAN_POINT('Ctrl Pts',(-1.38293909340318,-2.48335611964798,
1.64790782301531));
#15969=CARTESIAN_POINT('Ctrl Pts',(-1.45961750775132,-2.49243556329139,
1.57993091908226));
#15970=CARTESIAN_POINT('Ctrl Pts',(-1.53114165351361,-2.50151505675352,
1.50704173381545));
#15971=CARTESIAN_POINT('Ctrl Pts',(-1.63219781099869,-2.51434343395977,
1.40405691789381));
#15972=CARTESIAN_POINT('Ctrl Pts',(-1.72318285274175,-2.52717174276055,
1.29105843264262));
#15973=CARTESIAN_POINT('Ctrl Pts',(-1.80215132297835,-2.54000002688318,
1.17022486064862));
#15974=CARTESIAN_POINT('Ctrl Pts',(-1.87537003053102,-2.5518942725329,1.05818928564172));
#15975=CARTESIAN_POINT('Ctrl Pts',(-1.93825866804043,-2.56378849696735,
0.939416864259108));
#15976=CARTESIAN_POINT('Ctrl Pts',(-1.98921976954583,-2.57568273504094,
0.815636020431718));
#15977=CARTESIAN_POINT('Ctrl Pts',(-1.99322167356137,-2.5766167729189,0.805915683913724));
#15978=CARTESIAN_POINT('Ctrl Pts',(-1.99714999655,-2.57755081088096,0.796164462336127));
#15979=CARTESIAN_POINT('Ctrl Pts',(-2.00100395068832,-2.57848484894402,
0.786383193490234));
#15980=CARTESIAN_POINT('Ctrl Pts',(-2.00629831746431,-2.57976798307355,
0.772946182320367));
#15981=CARTESIAN_POINT('Ctrl Pts',(-2.01145137689601,-2.58105111671826,
0.759454900076632));
#15982=CARTESIAN_POINT('Ctrl Pts',(-2.01646120941697,-2.58233424995876,
0.745911650883031));
#15983=CARTESIAN_POINT('Ctrl Pts',(-2.07587033556421,-2.59755029245722,
0.585308956796785));
#15984=CARTESIAN_POINT('Ctrl Pts',(-2.11513693986626,-2.61276627811604,
0.417402205530998));
#15985=CARTESIAN_POINT('Ctrl Pts',(-2.13438726309228,-2.62798234140889,
0.247239058661555));
#15986=CARTESIAN_POINT('Ctrl Pts',(-2.14597254926331,-2.6371397173955,0.144830972880328));
#15987=CARTESIAN_POINT('Ctrl Pts',(-2.15030844243079,-2.64629712150046,
0.0416048035328496));
#15988=CARTESIAN_POINT('Ctrl Pts',(-2.14742535580896,-2.65545458303564,
-0.0613479590683571));
#15989=CARTESIAN_POINT('Ctrl Pts',(-2.14388349299061,-2.66670449563844,
-0.187825103092371));
#15990=CARTESIAN_POINT('Ctrl Pts',(-2.12943572662261,-2.67795431606019,
-0.314140136072367));
#15991=CARTESIAN_POINT('Ctrl Pts',(-2.10404000415043,-2.68920409851113,
-0.438193946100994));
#15992=CARTESIAN_POINT('Ctrl Pts',(-2.08093266461339,-2.69944017441315,
-0.551069392441806));
#15993=CARTESIAN_POINT('Ctrl Pts',(-2.04876210810997,-2.70967621887905,
-0.662071553421715));
#15994=CARTESIAN_POINT('Ctrl Pts',(-2.00753391608164,-2.71991227274539,
-0.769615212908264));
#15995=CARTESIAN_POINT('Ctrl Pts',(-1.99073561147467,-2.72408292254497,
-0.813433558116374));
#15996=CARTESIAN_POINT('Ctrl Pts',(-1.97243403118461,-2.72825357390515,
-0.856677792790132));
#15997=CARTESIAN_POINT('Ctrl Pts',(-1.9526992126251,-2.73242422958818,-0.899267183121456));
#15998=CARTESIAN_POINT('Ctrl Pts',(-1.90326331720604,-2.74287175904245,
-1.00595398340959));
#15999=CARTESIAN_POINT('Ctrl Pts',(-1.84489228968031,-2.75331932322472,
-1.10841690245437));
#16000=CARTESIAN_POINT('Ctrl Pts',(-1.77867028859895,-2.76376690339706,
-1.20553228931488));
#16001=CARTESIAN_POINT('Ctrl Pts',(-1.71025876617817,-2.77455991559136,
-1.30585863640679));
#16002=CARTESIAN_POINT('Ctrl Pts',(-1.63346781980748,-2.78535294485061,
-1.40047918676907));
#16003=CARTESIAN_POINT('Ctrl Pts',(-1.54944166015184,-2.79614597051608,
-1.48813545871277));
#16004=CARTESIAN_POINT('Ctrl Pts',(-1.51506181712427,-2.80056200630413,
-1.52400058550372));
#16005=CARTESIAN_POINT('Ctrl Pts',(-1.47947021694904,-2.80497804149054,
-1.55869950244843));
#16006=CARTESIAN_POINT('Ctrl Pts',(-1.44274333212728,-2.80939407466028,
-1.5921443698884));
#16007=CARTESIAN_POINT('Ctrl Pts',(-1.36675766648564,-2.8185305756602,-1.66133974344259));
#16008=CARTESIAN_POINT('Ctrl Pts',(-1.28581733678521,-2.82766704559732,
-1.72524726017498));
#16009=CARTESIAN_POINT('Ctrl Pts',(-1.20068636638464,-2.83680349751591,
-1.78296493675049));
#16010=CARTESIAN_POINT('Ctrl Pts',(-1.13642101631696,-2.84370060297778,
-1.82653599758493));
#16011=CARTESIAN_POINT('Ctrl Pts',(-1.06976858867396,-2.85059769817135,
-1.86658003345463));
#16012=CARTESIAN_POINT('Ctrl Pts',(-1.00107121872319,-2.85749478870825,
-1.90272342059117));
#16013=CARTESIAN_POINT('Ctrl Pts',(-0.910271969975343,-2.86661086752968,
-1.95049515335986));
#16014=CARTESIAN_POINT('Ctrl Pts',(-0.815900262721384,-2.8757269382161,
-1.99145060003429));
#16015=CARTESIAN_POINT('Ctrl Pts',(-0.719119978740421,-2.88484301372475,
-2.0254427242301));
#16016=CARTESIAN_POINT('Ctrl Pts',(-0.713739094553147,-2.88534985814116,
-2.02733265135217));
#16017=CARTESIAN_POINT('Ctrl Pts',(-0.708350768133567,-2.88585670257248,
-2.02920106606425));
#16018=CARTESIAN_POINT('Ctrl Pts',(-0.702955200467601,-2.88636354702093,
-2.03104794768616));
#16019=CARTESIAN_POINT('Ctrl Pts',(-0.598216337224688,-2.89620242119662,
-2.06689964923064));
#16020=CARTESIAN_POINT('Ctrl Pts',(-0.490737426444422,-2.90604137804317,
-2.09464568934945));
#16021=CARTESIAN_POINT('Ctrl Pts',(-0.38178492289613,-2.91588035490109,
-2.11417112339656));
#16022=CARTESIAN_POINT('Ctrl Pts',(-0.272214869587739,-2.92577509970926,
-2.13380722885295));
#16023=CARTESIAN_POINT('Ctrl Pts',(-0.161153117653703,-2.93566986475628,
-2.14512948741539));
#16024=CARTESIAN_POINT('Ctrl Pts',(-0.0498742561368832,-2.94556458631102,
-2.14797114567485));
#16025=CARTESIAN_POINT('Ctrl Pts',(0.0167371607961003,-2.95148755689082,
-2.14967215951093));
#16026=CARTESIAN_POINT('Ctrl Pts',(0.0834265370338267,-2.95741051188645,
-2.1483334293431));
#16027=CARTESIAN_POINT('Ctrl Pts',(0.149919701399027,-2.9633334376282,-2.14391022910733));
#16028=CARTESIAN_POINT('Ctrl Pts',(0.251021357348566,-2.97233913928601,
-2.13718483300531));
#16029=CARTESIAN_POINT('Ctrl Pts',(0.351700451929421,-2.98134483501702,
-2.12332085454694));
#16030=CARTESIAN_POINT('Ctrl Pts',(0.45082962216509,-2.99035053533562,-2.10217188848715));
#16031=CARTESIAN_POINT('Ctrl Pts',(0.468209302747445,-2.99192944691721,
-2.09846397613509));
#16032=CARTESIAN_POINT('Ctrl Pts',(0.485541342774309,-2.99350835863981,
-2.09453226464521));
#16033=CARTESIAN_POINT('Ctrl Pts',(0.502819678785445,-2.99508727056008,
-2.09037613140608));
#16034=CARTESIAN_POINT('Ctrl Pts',(0.601517176268586,-3.00410634827552,
-2.06663542225191));
#16035=CARTESIAN_POINT('Ctrl Pts',(0.698460834250939,-3.01312543244114,
-2.0355679225887));
#16036=CARTESIAN_POINT('Ctrl Pts',(0.792702219519714,-3.02214453361833,
-1.99780436319945));
#16037=CARTESIAN_POINT('Ctrl Pts',(0.855948223313822,-3.02819731081006,
-1.97246099400342));
#16038=CARTESIAN_POINT('Ctrl Pts',(0.917977434715979,-3.03425009566351,
-1.94410294380237));
#16039=CARTESIAN_POINT('Ctrl Pts',(0.978509859770852,-3.04030289137092,
-1.91293217178945));
#16040=CARTESIAN_POINT('Ctrl Pts',(1.08348604361805,-3.05079973491213,-1.85887538006963));
#16041=CARTESIAN_POINT('Ctrl Pts',(1.18409430990973,-3.06129660945067,-1.79629832428746));
#16042=CARTESIAN_POINT('Ctrl Pts',(1.2790534874194,-3.07179348120978,-1.72608240750692));
#16043=CARTESIAN_POINT('Ctrl Pts',(1.37191500981002,-3.08205847631034,-1.65741756542116));
#16044=CARTESIAN_POINT('Ctrl Pts',(1.45937529059133,-3.09232346875291,-1.58144670908853));
#16045=CARTESIAN_POINT('Ctrl Pts',(1.54020412886531,-3.1025884269501,-1.49895764141283));
#16046=CARTESIAN_POINT('Ctrl Pts',(1.57874687027005,-3.10748321002225,-1.45962322968509));
#16047=CARTESIAN_POINT('Ctrl Pts',(1.61578118376996,-3.11237798530769,-1.41880624933984));
#16048=CARTESIAN_POINT('Ctrl Pts',(1.65117000973465,-3.11727274938154,-1.37658999295121));
#16049=CARTESIAN_POINT('Ctrl Pts',(1.68828215808527,-3.12240587277567,-1.33231794020028));
#16050=CARTESIAN_POINT('Ctrl Pts',(1.72356791055107,-3.1275389907195,-1.28652619838855));
#16051=CARTESIAN_POINT('Ctrl Pts',(1.75686153146657,-3.13267210796456,-1.23932947979743));
#16052=CARTESIAN_POINT('Ctrl Pts',(1.82542896556432,-3.14324364295352,-1.14212894099627));
#16053=CARTESIAN_POINT('Ctrl Pts',(1.88554372347303,-3.15381517497873,-1.03896801995445));
#16054=CARTESIAN_POINT('Ctrl Pts',(1.93676088325265,-3.16438674554565,-0.931553000126708));
#16055=CARTESIAN_POINT('Ctrl Pts',(1.98497550482512,-3.17433857177936,-0.830435043674648));
#16056=CARTESIAN_POINT('Ctrl Pts',(2.02530530011653,-3.18429043216828,-0.725548422436352));
#16057=CARTESIAN_POINT('Ctrl Pts',(2.05742048141989,-3.19424236133786,-0.618324980965681));
#16058=CARTESIAN_POINT('Ctrl Pts',(2.10378205582973,-3.20860899686635,-0.46353689139319));
#16059=CARTESIAN_POINT('Ctrl Pts',(2.13314836674837,-3.22297550741097,-0.303496650724494));
#16060=CARTESIAN_POINT('Ctrl Pts',(2.14439073836144,-3.23734199227713,-0.14222435195816));
#16061=CARTESIAN_POINT('Ctrl Pts',(2.15297465656259,-3.24831127306355,-0.0190876804117314));
#16062=CARTESIAN_POINT('Ctrl Pts',(2.15099200706442,-3.2592805388799,0.104766880514908));
#16063=CARTESIAN_POINT('Ctrl Pts',(2.13792606424054,-3.27024983392955,0.227534928837607));
#16064=CARTESIAN_POINT('Ctrl Pts',(2.13754399199661,-3.2705705963292,0.231124892787152));
#16065=CARTESIAN_POINT('Ctrl Pts',(2.13715244165655,-3.27089135875384,0.234713926564423));
#16066=CARTESIAN_POINT('Ctrl Pts',(2.13675143309155,-3.27121212120459,0.238301988353448));
#16067=CARTESIAN_POINT('Ctrl Pts',(2.12006352161317,-3.28456060263571,0.387618643257629));
#16068=CARTESIAN_POINT('Ctrl Pts',(2.0870328714325,-3.29790904708474,0.534960049969257));
#16069=CARTESIAN_POINT('Ctrl Pts',(2.03925161079542,-3.31125752348132,0.67736934110968));
#16070=CARTESIAN_POINT('Ctrl Pts',(1.99519448295209,-3.32356560249129,0.8086790692792));
#16071=CARTESIAN_POINT('Ctrl Pts',(1.9385955017089,-3.33587370866286,0.935796635592113));
#16072=CARTESIAN_POINT('Ctrl Pts',(1.87066540489768,-3.34818189603184,1.05641555578819));
#16073=CARTESIAN_POINT('Ctrl Pts',(1.81420327390761,-3.35841221396306,1.1566715776649));
#16074=CARTESIAN_POINT('Ctrl Pts',(1.74981010065795,-3.36864246265313,1.25260873732792));
#16075=CARTESIAN_POINT('Ctrl Pts',(1.67816911246331,-3.37887267710189,1.34277188237266));
#16076=CARTESIAN_POINT('Ctrl Pts',(1.61058024014888,-3.38852425611483,1.42783527208108));
#16077=CARTESIAN_POINT('Ctrl Pts',(1.53654116992183,-3.39817580465036,1.50775846422047));
#16078=CARTESIAN_POINT('Ctrl Pts',(1.45666386721952,-3.40782735209894,1.58133816061886));
#16079=CARTESIAN_POINT('Ctrl Pts',(1.4088717163615,-3.41360206151039,1.62536233058195));
#16080=CARTESIAN_POINT('Ctrl Pts',(1.35899025659116,-3.41937677053273,1.66711606163006));
#16081=CARTESIAN_POINT('Ctrl Pts',(1.30728661284953,-3.42515148546112,1.70648898569144));
#16082=CARTESIAN_POINT('Ctrl Pts',(1.21683432243152,-3.43525398799254,1.7753694533738));
#16083=CARTESIAN_POINT('Ctrl Pts',(1.12087575786482,-3.44535654774423,1.83691690101427));
#16084=CARTESIAN_POINT('Ctrl Pts',(1.02072745743775,-3.45545912633785,1.8906623281449));
#16085=CARTESIAN_POINT('Ctrl Pts',(0.918166962665796,-3.46580503789717,
1.94570227964423));
#16086=CARTESIAN_POINT('Ctrl Pts',(0.811211277586695,-3.47615096921703,
1.99256053397001));
#16087=CARTESIAN_POINT('Ctrl Pts',(0.701240761208127,-3.48649687907851,
2.03069136304103));
#16088=CARTESIAN_POINT('Ctrl Pts',(0.645881247179067,-3.4917050436028,2.04988654586285));
#16089=CARTESIAN_POINT('Ctrl Pts',(0.589757320139156,-3.49691320268921,
2.06686934936848));
#16090=CARTESIAN_POINT('Ctrl Pts',(0.533043472824269,-3.50212135107947,
2.08156541081787));
#16091=CARTESIAN_POINT('Ctrl Pts',(0.435417063012063,-3.51108658361408,
2.10686300189326));
#16092=CARTESIAN_POINT('Ctrl Pts',(0.335946159210999,-3.52005179614604,
2.12540431829036));
#16093=CARTESIAN_POINT('Ctrl Pts',(0.235664798255475,-3.52901699808759,
2.13674789347885));
#16094=CARTESIAN_POINT('Ctrl Pts',(0.174528790778321,-3.5344825865849,2.143663444793));
#16095=CARTESIAN_POINT('Ctrl Pts',(0.11309205425833,-3.53994817114611,2.14790472408161));
#16096=CARTESIAN_POINT('Ctrl Pts',(0.0515913436216816,-3.5454137539039,
2.14938091862104));
#16097=CARTESIAN_POINT('Ctrl Pts',(-0.0491838684249719,-3.55436967092784,
2.15179981453611));
#16098=CARTESIAN_POINT('Ctrl Pts',(-0.150130148628519,-3.56332558310961,
2.14679170622627));
#16099=CARTESIAN_POINT('Ctrl Pts',(-0.250189782466457,-3.5722814998323,
2.13472144525996));
#16100=CARTESIAN_POINT('Ctrl Pts',(-0.275548643893186,-3.57455126479554,
2.13166238874048));
#16101=CARTESIAN_POINT('Ctrl Pts',(-0.300850603572711,-3.57682103005044,
2.12814998377674));
#16102=CARTESIAN_POINT('Ctrl Pts',(-0.326078579897805,-3.57909079574975,
2.12419068029949));
#16103=CARTESIAN_POINT('Ctrl Pts',(-0.436100150534687,-3.58898945682339,
2.10692378653116));
#16104=CARTESIAN_POINT('Ctrl Pts',(-0.544767060932894,-3.59888819610816,
2.08115384518473));
#16105=CARTESIAN_POINT('Ctrl Pts',(-0.65087082904308,-3.60878695149005,
2.04733995937731));
#16106=CARTESIAN_POINT('Ctrl Pts',(-0.756777976652686,-3.61866736352493,
2.01358873395672));
#16107=CARTESIAN_POINT('Ctrl Pts',(-0.860132761081111,-3.62854779159731,
1.97182287975362));
#16108=CARTESIAN_POINT('Ctrl Pts',(-0.959720255848221,-3.63842817393778,
1.92244995048172));
#16109=CARTESIAN_POINT('Ctrl Pts',(-1.01896167856859,-3.64430569810123,
1.89307957038752));
#16110=CARTESIAN_POINT('Ctrl Pts',(-1.07686963551438,-3.65018320608162,
1.86101638968194));
#16111=CARTESIAN_POINT('Ctrl Pts',(-1.13318331580902,-3.65606068487622,
1.82633897465691));
#16112=CARTESIAN_POINT('Ctrl Pts',(-1.21923957158997,-3.66504240682813,
1.77334637176535));
#16113=CARTESIAN_POINT('Ctrl Pts',(-1.30156902058835,-3.67402412301627,
1.71424500772037));
#16114=CARTESIAN_POINT('Ctrl Pts',(-1.37911670791559,-3.68300584746048,
1.64940507645279));
#16115=CARTESIAN_POINT('Ctrl Pts',(-1.45890924686097,-3.69224757499889,
1.58268815788047));
#16116=CARTESIAN_POINT('Ctrl Pts',(-1.53363805546767,-3.70148931127831,
1.50989612163114));
#16117=CARTESIAN_POINT('Ctrl Pts',(-1.60269510276803,-3.71073107157176,
1.43208165791051));
#16118=CARTESIAN_POINT('Ctrl Pts',(-1.65823669784161,-3.71816408714443,
1.36949659811146));
#16119=CARTESIAN_POINT('Ctrl Pts',(-1.71010990385534,-3.72559711825116,
1.30366373156248));
#16120=CARTESIAN_POINT('Ctrl Pts',(-1.75801902860842,-3.7330301728381,1.23514382748167));
#16121=CARTESIAN_POINT('Ctrl Pts',(-1.8292633322244,-3.7440836579626,1.13324981720219));
#16122=CARTESIAN_POINT('Ctrl Pts',(-1.89185880350952,-3.75513714094056,
1.0252604177841));
#16123=CARTESIAN_POINT('Ctrl Pts',(-1.94489966990501,-3.76619061134567,
0.912769160216455));
#16124=CARTESIAN_POINT('Ctrl Pts',(-1.99619038500844,-3.7768793583436,0.803989695708698));
#16125=CARTESIAN_POINT('Ctrl Pts',(-2.03854705782826,-3.7875680935847,0.690999271567748));
#16126=CARTESIAN_POINT('Ctrl Pts',(-2.07110465120936,-3.79825680764115,
0.575226138231553));
#16127=CARTESIAN_POINT('Ctrl Pts',(-2.08302783918947,-3.80217121081797,
0.532827892892737));
#16128=CARTESIAN_POINT('Ctrl Pts',(-2.09363632692981,-3.80608561115359,
0.490056409623361));
#16129=CARTESIAN_POINT('Ctrl Pts',(-2.10288583604143,-3.81000000818494,
0.446981897454489));
#16130=CARTESIAN_POINT('Ctrl Pts',(-2.11122461550155,-3.8135289839576,0.408148608790789));
#16131=CARTESIAN_POINT('Ctrl Pts',(-2.1184553833498,-3.81705795633114,0.369084721521393));
#16132=CARTESIAN_POINT('Ctrl Pts',(-2.12454729965618,-3.82058692703921,
0.329846588021416));
#16133=CARTESIAN_POINT('Ctrl Pts',(-2.14500360606005,-3.83243700876457,
0.198087180763822));
#16134=CARTESIAN_POINT('Ctrl Pts',(-2.15261465112136,-3.84428707171052,
0.0643636641716998));
#16135=CARTESIAN_POINT('Ctrl Pts',(-2.14789672175115,-3.85613718151895,
-0.0689357913238956));
#16136=CARTESIAN_POINT('Ctrl Pts',(-2.14380492206176,-3.86641462991389,
-0.184544701036669));
#16137=CARTESIAN_POINT('Ctrl Pts',(-2.13044038557123,-3.87669211355817,
-0.299833970567715));
#16138=CARTESIAN_POINT('Ctrl Pts',(-2.10816907223884,-3.88696967527413,
-0.413258423524959));
#16139=CARTESIAN_POINT('Ctrl Pts',(-2.07723123887715,-3.90124658328524,
-0.57082016101039));
#16140=CARTESIAN_POINT('Ctrl Pts',(-2.02902853462656,-3.91552334561718,
-0.725184703687629));
#16141=CARTESIAN_POINT('Ctrl Pts',(-1.96432556990801,-3.92980007738602,
-0.872244774834655));
#16142=CARTESIAN_POINT('Ctrl Pts',(-1.92147496314573,-3.93925507873779,
-0.969637735212349));
#16143=CARTESIAN_POINT('Ctrl Pts',(-1.87138840711967,-3.94871006668468,
-1.06382611877347));
#16144=CARTESIAN_POINT('Ctrl Pts',(-1.81429901500113,-3.95816507466421,
-1.15361132284044));
#16145=CARTESIAN_POINT('Ctrl Pts',(-1.80267723264998,-3.96008984633874,
-1.17188904592168));
#16146=CARTESIAN_POINT('Ctrl Pts',(-1.7907652699902,-3.96201461884347,-1.18998428708905));
#16147=CARTESIAN_POINT('Ctrl Pts',(-1.77857117794315,-3.96393939246046,
-1.20789076769297));
#16148=CARTESIAN_POINT('Ctrl Pts',(-1.70631579042681,-3.97534452726184,
-1.31399458338486));
#16149=CARTESIAN_POINT('Ctrl Pts',(-1.62427072861909,-3.98674965866473,
-1.41330788790257));
#16150=CARTESIAN_POINT('Ctrl Pts',(-1.5341310047501,-3.9981548057651,-1.50464901891823));
#16151=CARTESIAN_POINT('Ctrl Pts',(-1.43944800007175,-4.01013480248477,
-1.60059398484525));
#16152=CARTESIAN_POINT('Ctrl Pts',(-1.33583295329178,-4.02211481652421,
-1.68774399261372));
#16153=CARTESIAN_POINT('Ctrl Pts',(-1.22519919519716,-4.03409487001487,
-1.76470626599637));
#16154=CARTESIAN_POINT('Ctrl Pts',(-1.20422281494436,-4.03636631194902,
-1.77929846587639));
#16155=CARTESIAN_POINT('Ctrl Pts',(-1.18299400113378,-4.0386377553014,-1.79352433457489));
#16156=CARTESIAN_POINT('Ctrl Pts',(-1.16152564269842,-4.04090920022285,
-1.80737423761186));
#16157=CARTESIAN_POINT('Ctrl Pts',(-1.07059808751356,-4.05052972775721,
-1.8660344200609));
#16158=CARTESIAN_POINT('Ctrl Pts',(-0.975233856793274,-4.06015020406865,
-1.91803505472432));
#16159=CARTESIAN_POINT('Ctrl Pts',(-0.876496392399245,-4.06977065219613,
-1.96253168699072));
#16160=CARTESIAN_POINT('Ctrl Pts',(-0.787640766643975,-4.07842826705043,
-2.00257500923217));
#16161=CARTESIAN_POINT('Ctrl Pts',(-0.696054456911158,-4.08708585907987,
-2.03654116909533));
#16162=CARTESIAN_POINT('Ctrl Pts',(-0.602532959552935,-4.09574344507526,
-2.06384447888001));
#16163=CARTESIAN_POINT('Ctrl Pts',(-0.522829227727489,-4.10312187604487,
-2.08711373506707));
#16164=CARTESIAN_POINT('Ctrl Pts',(-0.441720492063881,-4.11050030263179,
-2.10554402195451));
#16165=CARTESIAN_POINT('Ctrl Pts',(-0.359817555710095,-4.11787873522977,
-2.11917939160544));
#16166=CARTESIAN_POINT('Ctrl Pts',(-0.24975524404404,-4.12779397617666,
-2.13750279209648));
#16167=CARTESIAN_POINT('Ctrl Pts',(-0.138301660871375,-4.1377092906271,
-2.14716746504687));
#16168=CARTESIAN_POINT('Ctrl Pts',(-0.0267587316605952,-4.14762462594713,
-2.14832538881259));
#16169=CARTESIAN_POINT('Ctrl Pts',(0.0865866807360727,-4.1577001885924,
-2.1495020241016));
#16170=CARTESIAN_POINT('Ctrl Pts',(0.200025723302156,-4.16777577278721,
-2.14189478402756));
#16171=CARTESIAN_POINT('Ctrl Pts',(0.312200346981725,-4.17785132330444,
-2.12561083565466));
#16172=CARTESIAN_POINT('Ctrl Pts',(0.37527943382547,-4.18351710140315,-2.11645389302468));
#16173=CARTESIAN_POINT('Ctrl Pts',(0.437958720801109,-4.18918286885252,
-2.10455231092883));
#16174=CARTESIAN_POINT('Ctrl Pts',(0.499995277943403,-4.19484861583228,
-2.08991802219758));
#16175=CARTESIAN_POINT('Ctrl Pts',(0.597528552581938,-4.20375624839063,
-2.06691013511109));
#16176=CARTESIAN_POINT('Ctrl Pts',(0.69354183936608,-4.21266386910625,-2.03712587047305));
#16177=CARTESIAN_POINT('Ctrl Pts',(0.786932036352475,-4.22157148620242,
-2.00063394444371));
#16178=CARTESIAN_POINT('Ctrl Pts',(0.828036981668865,-4.22549210234257,
-1.98457231621795));
#16179=CARTESIAN_POINT('Ctrl Pts',(0.868633832481699,-4.22941271778155,
-1.96721191752031));
#16180=CARTESIAN_POINT('Ctrl Pts',(0.90862926159499,-4.23333333322053,-1.94856174266362));
#16181=CARTESIAN_POINT('Ctrl Pts',(0.999498644208469,-4.24224094872318,
-1.90618865372738));
#16182=CARTESIAN_POINT('Ctrl Pts',(1.08726144411594,-4.25114856422586,-1.85715487810709));
#16183=CARTESIAN_POINT('Ctrl Pts',(1.17114146098775,-4.26005618795191,-1.80224348783637));
#16184=CARTESIAN_POINT('Ctrl Pts',(1.20806057760194,-4.26397680708578,-1.77807467985973));
#16185=CARTESIAN_POINT('Ctrl Pts',(1.24422788683378,-4.26789742781272,-1.75276780321408));
#16186=CARTESIAN_POINT('Ctrl Pts',(1.27957931791511,-4.27181805083389,-1.72639201418339));
#16187=CARTESIAN_POINT('Ctrl Pts',(1.3702680503316,-4.28187581430195,-1.65872892953555));
#16188=CARTESIAN_POINT('Ctrl Pts',(1.4556635312844,-4.29193364227575,-1.5839813747478));
#16189=CARTESIAN_POINT('Ctrl Pts',(1.53483475315364,-4.3019914798193,-1.5031378542605));
#16190=CARTESIAN_POINT('Ctrl Pts',(1.61323645562851,-4.31195155834294,-1.42308010738455));
#16191=CARTESIAN_POINT('Ctrl Pts',(1.68553520674605,-4.32191164625115,-1.33704328383143));
#16192=CARTESIAN_POINT('Ctrl Pts',(1.75079126578976,-4.33187169019429,-1.24595250185277));
#16193=CARTESIAN_POINT('Ctrl Pts',(1.78773523357387,-4.33751045459343,-1.19438250261951));
#16194=CARTESIAN_POINT('Ctrl Pts',(1.8224212065658,-4.3431492049012,-1.14119209659256));
#16195=CARTESIAN_POINT('Ctrl Pts',(1.85467186346985,-4.34878793143707,-1.08654601653875));
#16196=CARTESIAN_POINT('Ctrl Pts',(1.89687275700405,-4.3561663640351,-1.01504008060466));
#16197=CARTESIAN_POINT('Ctrl Pts',(1.93489002847075,-4.36354479062205,-0.94106042430691));
#16198=CARTESIAN_POINT('Ctrl Pts',(1.96829731533633,-4.37092322159169,-0.865046633882483));
#16199=CARTESIAN_POINT('Ctrl Pts',(2.01185562744538,-4.38054363765073,-0.765935550087445));
#16200=CARTESIAN_POINT('Ctrl Pts',(2.04757471480282,-4.39016406116053,-0.663366408448736));
#16201=CARTESIAN_POINT('Ctrl Pts',(2.07537116398524,-4.39978451516008,-0.558692542423503));
#16202=CARTESIAN_POINT('Ctrl Pts',(2.10038569014399,-4.40844213529894,-0.464494641726159));
#16203=CARTESIAN_POINT('Ctrl Pts',(2.11898467097047,-4.41709978012996,-0.368593231105418));
#16204=CARTESIAN_POINT('Ctrl Pts',(2.13114328281877,-4.42575746644398,-0.271977501874224));
#16205=CARTESIAN_POINT('Ctrl Pts',(2.14799668867745,-4.43775813749655,-0.138055626796601));
#16206=CARTESIAN_POINT('Ctrl Pts',(2.15251713901127,-4.44975876475148,-0.00250973760409071));
#16207=CARTESIAN_POINT('Ctrl Pts',(2.14455054625308,-4.46175937045459,0.132288978275308));
#16208=CARTESIAN_POINT('Ctrl Pts',(2.13696358465177,-4.47318811263152,0.260664145969383));
#16209=CARTESIAN_POINT('Ctrl Pts',(2.11805102970323,-4.48461683526174,0.38836291944513));
#16210=CARTESIAN_POINT('Ctrl Pts',(2.08763593327636,-4.49604555756,0.513320113310582));
#16211=CARTESIAN_POINT('Ctrl Pts',(2.08170861414705,-4.49827279640717,0.537671874526404));
#16212=CARTESIAN_POINT('Ctrl Pts',(2.07534431290476,-4.50050003524172,0.561919428162025));
#16213=CARTESIAN_POINT('Ctrl Pts',(2.06854152661343,-4.50272727420588,0.586047348227131));
#16214=CARTESIAN_POINT('Ctrl Pts',(2.06266257793018,-4.50465204782288,0.606898628544018));
#16215=CARTESIAN_POINT('Ctrl Pts',(2.05645768099176,-4.50657682032761,0.627655118162937));
#16216=CARTESIAN_POINT('Ctrl Pts',(2.04992647049026,-4.50850159200216,0.648306613882153));
#16217=CARTESIAN_POINT('Ctrl Pts',(2.00148207209989,-4.52277833377783,0.80148637829951));
#16218=CARTESIAN_POINT('Ctrl Pts',(1.93508341248904,-4.53705502987922,0.94888612204242));
#16219=CARTESIAN_POINT('Ctrl Pts',(1.85337829407576,-4.55133179542225,1.0872462190929));
#16220=CARTESIAN_POINT('Ctrl Pts',(1.79926773028061,-4.560786819143,1.17887747798519));
#16221=CARTESIAN_POINT('Ctrl Pts',(1.73844424393401,-4.57024187332064,1.26654474140526));
#16222=CARTESIAN_POINT('Ctrl Pts',(1.67167927767296,-4.57969699139271,1.34931380870346));
#16223=CARTESIAN_POINT('Ctrl Pts',(1.58800174988501,-4.59154723186343,1.45304951496815));
#16224=CARTESIAN_POINT('Ctrl Pts',(1.4948126152933,-4.60339736854122,1.54930761273379));
#16225=CARTESIAN_POINT('Ctrl Pts',(1.39356918635948,-4.61524746706802,1.6361369566103));
#16226=CARTESIAN_POINT('Ctrl Pts',(1.30576205774412,-4.62552490567718,1.71144293395264));
#16227=CARTESIAN_POINT('Ctrl Pts',(1.21189793087447,-4.63580231558964,1.77965629821637));
#16228=CARTESIAN_POINT('Ctrl Pts',(1.11295553457626,-4.64607973962771,1.83951895292272));
#16229=CARTESIAN_POINT('Ctrl Pts',(1.07898157212933,-4.64960871033575,1.86007406032922));
#16230=CARTESIAN_POINT('Ctrl Pts',(1.04440905037871,-4.65313768270927,1.87964475352249));
#16231=CARTESIAN_POINT('Ctrl Pts',(1.00930096127305,-4.65666665848189,1.89821843465103));
#16232=CARTESIAN_POINT('Ctrl Pts',(0.903387473349617,-4.66731281275567,
1.95425120094545));
#16233=CARTESIAN_POINT('Ctrl Pts',(0.79273223753515,-4.67795899147102,2.00114538521535));
#16234=CARTESIAN_POINT('Ctrl Pts',(0.678977839651301,-4.68860518531224,
2.03866324799128));
#16235=CARTESIAN_POINT('Ctrl Pts',(0.560988748976523,-4.69964770106407,
2.07757777433349));
#16236=CARTESIAN_POINT('Ctrl Pts',(0.439664173613485,-4.71069023308892,
2.10640542715997));
#16237=CARTESIAN_POINT('Ctrl Pts',(0.316807093101287,-4.72173277099149,
2.12483465690906));
#16238=CARTESIAN_POINT('Ctrl Pts',(0.272660948818338,-4.72570067800559,
2.13145681846568));
#16239=CARTESIAN_POINT('Ctrl Pts',(0.228316755754743,-4.7296685857786,2.13673590012991));
#16240=CARTESIAN_POINT('Ctrl Pts',(0.183857783687548,-4.73363649382823,
2.14065585624885));
#16241=CARTESIAN_POINT('Ctrl Pts',(0.0803066645080147,-4.74287830262938,
2.14978597834517));
#16242=CARTESIAN_POINT('Ctrl Pts',(-0.0240018215168891,-4.75212007513271,
2.15155020610059));
#16243=CARTESIAN_POINT('Ctrl Pts',(-0.127875392181151,-4.7613618266112,
2.14569602543938));
#16244=CARTESIAN_POINT('Ctrl Pts',(-0.211419418846149,-4.76879483509461,
2.14098759169503));
#16245=CARTESIAN_POINT('Ctrl Pts',(-0.294681391670819,-4.77622782997754,
2.13135186522761));
#16246=CARTESIAN_POINT('Ctrl Pts',(-0.37703846110927,-4.78366081920613,
2.11668183700904));
#16247=CARTESIAN_POINT('Ctrl Pts',(-0.476555422722861,-4.79264254365043,
2.09895516648698));
#16248=CARTESIAN_POINT('Ctrl Pts',(-0.574750043958772,-4.80162425983865,
2.07387677410038));
#16249=CARTESIAN_POINT('Ctrl Pts',(-0.670660627882294,-4.81060598179061,
2.04201684610747));
#16250=CARTESIAN_POINT('Ctrl Pts',(-0.775749929386506,-4.82044726152873,
2.00710789819179));
#16251=CARTESIAN_POINT('Ctrl Pts',(-0.878098236304415,-4.83028862309304,
1.96406650285739));
#16252=CARTESIAN_POINT('Ctrl Pts',(-0.976634154300157,-4.8401300054433,
1.91358292833901));
#16253=CARTESIAN_POINT('Ctrl Pts',(-1.07602185190398,-4.85005646021153,
1.8626629558026));
#16254=CARTESIAN_POINT('Ctrl Pts',(-1.17153217597132,-4.85998293612661,
1.80417094133948));
#16255=CARTESIAN_POINT('Ctrl Pts',(-1.26204688891126,-4.86990937055149,
1.73876672548302));
#16256=CARTESIAN_POINT('Ctrl Pts',(-1.31574469854142,-4.8757982229683,1.69996570609074));
#16257=CARTESIAN_POINT('Ctrl Pts',(-1.36768388313526,-4.88168706078284,
1.65873109857275));
#16258=CARTESIAN_POINT('Ctrl Pts',(-1.41762519582607,-4.88757587091708,
1.61519413405892));
#16259=CARTESIAN_POINT('Ctrl Pts',(-1.49357778596525,-4.89653179054423,
1.54898151281495));
#16260=CARTESIAN_POINT('Ctrl Pts',(-1.56493859108713,-4.90548770325245,
1.4774108413));
#16261=CARTESIAN_POINT('Ctrl Pts',(-1.63074006771737,-4.91444361842479,
1.40104746702544));
#16262=CARTESIAN_POINT('Ctrl Pts',(-1.64741662811824,-4.91671338299491,
1.38169412590424));
#16263=CARTESIAN_POINT('Ctrl Pts',(-1.66373626609291,-4.9189831477233,1.36203315505184));
#16264=CARTESIAN_POINT('Ctrl Pts',(-1.679683585303,-4.9212529127627,1.34207416089156));
#16265=CARTESIAN_POINT('Ctrl Pts',(-1.7426728306755,-4.93021810528952,1.26323946999538));
#16266=CARTESIAN_POINT('Ctrl Pts',(-1.79984989259213,-4.93918330266859,
1.17975311248381));
#16267=CARTESIAN_POINT('Ctrl Pts',(-1.85085912733998,-4.94814851431222,
1.09267833389976));
#16268=CARTESIAN_POINT('Ctrl Pts',(-1.88195664065002,-4.95361410872455,
1.03959365032485));
#16269=CARTESIAN_POINT('Ctrl Pts',(-1.91076264313262,-4.95907970843854,
0.985175881641332));
#16270=CARTESIAN_POINT('Ctrl Pts',(-1.93720535570157,-4.96454531558686,
0.929669464527957));
#16271=CARTESIAN_POINT('Ctrl Pts',(-1.98722787292446,-4.97488477781101,
0.82466621651417));
#16272=CARTESIAN_POINT('Ctrl Pts',(-2.02885485523213,-4.98522428219098,
0.715652303906996));
#16273=CARTESIAN_POINT('Ctrl Pts',(-2.06164273452908,-4.99556378758447,
0.604041827372011));
#16274=CARTESIAN_POINT('Ctrl Pts',(-2.09383013986182,-5.00571393630334,
0.494475374016633));
#16275=CARTESIAN_POINT('Ctrl Pts',(-2.1174995142741,-5.01586408599892,0.382405247350599));
#16276=CARTESIAN_POINT('Ctrl Pts',(-2.13218356424474,-5.02601419774826,
0.269158197582545));
#16277=CARTESIAN_POINT('Ctrl Pts',(-2.13965861246377,-5.03118120377906,
0.211508764396793));
#16278=CARTESIAN_POINT('Ctrl Pts',(-2.14480439931278,-5.03634819997643,
0.153554287072376));
#16279=CARTESIAN_POINT('Ctrl Pts',(-2.14755404178161,-5.04151518120572,
0.0954703307314682));
#16280=CARTESIAN_POINT('Ctrl Pts',(-2.1506270936678,-5.04728989613413,0.0305546140104575));
#16281=CARTESIAN_POINT('Ctrl Pts',(-2.15070506431235,-5.0530646051565,-0.0344955820371225));
#16282=CARTESIAN_POINT('Ctrl Pts',(-2.147700795961,-5.05883931456796,-0.0994046846055585));
#16283=CARTESIAN_POINT('Ctrl Pts',(-2.14237858720656,-5.06906949556035,
-0.214394343827251));
#16284=CARTESIAN_POINT('Ctrl Pts',(-2.12738017659775,-5.07929967777391,
-0.328940292500448));
#16285=CARTESIAN_POINT('Ctrl Pts',(-2.1033362720808,-5.08952989620844,-0.441563566451724));
#16286=CARTESIAN_POINT('Ctrl Pts',(-2.08065232489935,-5.09918147898111,
-0.547816708320187));
#16287=CARTESIAN_POINT('Ctrl Pts',(-2.04991806394045,-5.10883309399318,
-0.652357606947935));
#16288=CARTESIAN_POINT('Ctrl Pts',(-2.01170181027345,-5.11848477063517,
-0.753962008416238));
#16289=CARTESIAN_POINT('Ctrl Pts',(-1.95884744412238,-5.13183336455158,
-0.894484318231309));
#16290=CARTESIAN_POINT('Ctrl Pts',(-1.89157103852933,-5.14518186296322,
-1.0297108192664));
#16291=CARTESIAN_POINT('Ctrl Pts',(-1.81113280530604,-5.15853033479973,
-1.15656558152439));
#16292=CARTESIAN_POINT('Ctrl Pts',(-1.73696403125853,-5.17083840960258,
-1.27353312073731));
#16293=CARTESIAN_POINT('Ctrl Pts',(-1.65160455740265,-5.18314646181149,
-1.38338351355141));
#16294=CARTESIAN_POINT('Ctrl Pts',(-1.5560272601333,-5.19545454546225,-1.48366899616924));
#16295=CARTESIAN_POINT('Ctrl Pts',(-1.55353640867527,-5.19577530791299,
-1.48628254821282));
#16296=CARTESIAN_POINT('Ctrl Pts',(-1.55103873300124,-5.19609607033762,
-1.48888947961775));
#16297=CARTESIAN_POINT('Ctrl Pts',(-1.54853425237114,-5.19641683273726,
-1.49148974828301));
#16298=CARTESIAN_POINT('Ctrl Pts',(-1.43636203427787,-5.2107833362814,-1.60795217978105));
#16299=CARTESIAN_POINT('Ctrl Pts',(-1.31054382535276,-5.22514978968107,
-1.7110490773328));
#16300=CARTESIAN_POINT('Ctrl Pts',(-1.17492438881865,-5.23951629224171,
-1.7990638690772));
#16301=CARTESIAN_POINT('Ctrl Pts',(-1.07137451604925,-5.25048558654283,
-1.86626603950257));
#16302=CARTESIAN_POINT('Ctrl Pts',(-0.962109293889222,-5.26145490950394,
-1.9246757010747));
#16303=CARTESIAN_POINT('Ctrl Pts',(-0.84881997766153,-5.27242430532847,
-1.97352716347531));
#16304=CARTESIAN_POINT('Ctrl Pts',(-0.739638176970612,-5.28299598524052,
-2.02060742495879));
#16305=CARTESIAN_POINT('Ctrl Pts',(-0.626517694921249,-5.29356758753868,
-2.0588913811808));
#16306=CARTESIAN_POINT('Ctrl Pts',(-0.511028391401235,-5.3041391537284,
-2.08757984687915));
#16307=CARTESIAN_POINT('Ctrl Pts',(-0.402309495430654,-5.31409097584348,
-2.11458648924993));
#16308=CARTESIAN_POINT('Ctrl Pts',(-0.291492680525968,-5.3240427659596,
-2.1330895639489));
#16309=CARTESIAN_POINT('Ctrl Pts',(-0.179907363169104,-5.33399455870215,
-2.14245964744254));
#16310=CARTESIAN_POINT('Ctrl Pts',(-0.122351852152804,-5.33912767594726,
-2.14729272007715));
#16311=CARTESIAN_POINT('Ctrl Pts',(-0.064592098313675,-5.34426079389113,
-2.14969662974198));
#16312=CARTESIAN_POINT('Ctrl Pts',(-0.00682250918969845,-5.34939391728529,
-2.14972460168947));
#16313=CARTESIAN_POINT('Ctrl Pts',(0.108166914391305,-5.35961131556033,
-2.14978027939405));
#16314=CARTESIAN_POINT('Ctrl Pts',(0.223093636218288,-5.36982876268752,
-2.14042775114858));
#16315=CARTESIAN_POINT('Ctrl Pts',(0.336579295018667,-5.3800462275161,-2.12212138775708));
#16316=CARTESIAN_POINT('Ctrl Pts',(0.45318559989502,-5.39054465376185,-2.10331163317337));
#16317=CARTESIAN_POINT('Ctrl Pts',(0.56827187342757,-5.40104309869592,-2.0750486851374));
#16318=CARTESIAN_POINT('Ctrl Pts',(0.680345080826755,-5.41154152852646,
-2.03777130715719));
#16319=CARTESIAN_POINT('Ctrl Pts',(0.733088785761198,-5.41648228196884,
-2.02022789004132));
#16320=CARTESIAN_POINT('Ctrl Pts',(0.785165052028643,-5.42142303206607,
-2.00068719241862));
#16321=CARTESIAN_POINT('Ctrl Pts',(0.836417046445954,-5.42636377529591,
-1.97919113881164));
#16322=CARTESIAN_POINT('Ctrl Pts',(0.929975508341221,-5.43538290406268,
-1.93995095440218));
#16323=CARTESIAN_POINT('Ctrl Pts',(1.02088553759679,-5.44440200873009,-1.8941483086934));
#16324=CARTESIAN_POINT('Ctrl Pts',(1.10804186902105,-5.4534210998595,-1.84207162275567));
#16325=CARTESIAN_POINT('Ctrl Pts',(1.16653304731231,-5.45947387030836,-1.80712262166504));
#16326=CARTESIAN_POINT('Ctrl Pts',(1.22333370305523,-5.46552663465992,-1.76934898144453));
#16327=CARTESIAN_POINT('Ctrl Pts',(1.27811476006261,-5.47157939610642,-1.72885009767664));
#16328=CARTESIAN_POINT('Ctrl Pts',(1.35962167103746,-5.48058509835686,-1.66859315678911));
#16329=CARTESIAN_POINT('Ctrl Pts',(1.43665565945691,-5.48959079417627,-1.60230184066544));
#16330=CARTESIAN_POINT('Ctrl Pts',(1.50859729941936,-5.49859649407912,-1.53092790094143));
#16331=CARTESIAN_POINT('Ctrl Pts',(1.52121036497895,-5.50017540558772,-1.51841436661758));
#16332=CARTESIAN_POINT('Ctrl Pts',(1.53366699810796,-5.50175431722184,-1.50574468538882));
#16333=CARTESIAN_POINT('Ctrl Pts',(1.54596399104637,-5.50333322903814,-1.49292408572141));
#16334=CARTESIAN_POINT('Ctrl Pts',(1.62278259204332,-5.51319659949247,-1.41283454388587));
#16335=CARTESIAN_POINT('Ctrl Pts',(1.69340018429812,-5.52306005107312,-1.3268320665492));
#16336=CARTESIAN_POINT('Ctrl Pts',(1.75715433925784,-5.53292352065149,-1.2360112097772));
#16337=CARTESIAN_POINT('Ctrl Pts',(1.82098380056235,-5.54279864095037,-1.14508307549899));
#16338=CARTESIAN_POINT('Ctrl Pts',(1.87793435093592,-5.55267377928949,-1.04932402499391));
#16339=CARTESIAN_POINT('Ctrl Pts',(1.92730132974581,-5.56254887231616,-0.949800550051649));
#16340=CARTESIAN_POINT('Ctrl Pts',(1.95688676024052,-5.56846697557897,-0.890156534527914));
#16341=CARTESIAN_POINT('Ctrl Pts',(1.98374769198347,-5.57438506256756,-0.829159971897384));
#16342=CARTESIAN_POINT('Ctrl Pts',(2.0077238870586,-5.5803031196459,-0.767037530372227));
#16343=CARTESIAN_POINT('Ctrl Pts',(2.04465641671103,-5.58941919573078,-0.671345161065114));
#16344=CARTESIAN_POINT('Ctrl Pts',(2.07474324568416,-5.59853526627298,-0.572967749687063));
#16345=CARTESIAN_POINT('Ctrl Pts',(2.09734624033654,-5.60765134422977,-0.472890201266301));
#16346=CARTESIAN_POINT('Ctrl Pts',(2.09860294357747,-5.60815818878241,-0.467325992568302));
#16347=CARTESIAN_POINT('Ctrl Pts',(2.09983652484205,-5.60866503335797,-0.461756533546821));
#16348=CARTESIAN_POINT('Ctrl Pts',(2.10104687894532,-5.60917187795868,-0.456181995147292));
#16349=CARTESIAN_POINT('Ctrl Pts',(2.12286484469567,-5.61830831010622,-0.355694800907008));
#16350=CARTESIAN_POINT('Ctrl Pts',(2.13713093076308,-5.62744475042515,-0.253556656199974));
#16351=CARTESIAN_POINT('Ctrl Pts',(2.14400573572527,-5.63658121195977,-0.150935426994296));
#16352=CARTESIAN_POINT('Ctrl Pts',(2.14919552441782,-5.64347832468125,-0.0734666845532049));
#16353=CARTESIAN_POINT('Ctrl Pts',(2.15017435337808,-5.65037544949297,0.00427695486709702));
#16354=CARTESIAN_POINT('Ctrl Pts',(2.14703088504541,-5.65727259200655,0.0817948386269175));
#16355=CARTESIAN_POINT('Ctrl Pts',(2.1421091136896,-5.66807154235945,0.203165649297445));
#16356=CARTESIAN_POINT('Ctrl Pts',(2.1270823894308,-5.678870504772,0.324156550535808));
#16357=CARTESIAN_POINT('Ctrl Pts',(2.10220051973105,-5.68966945855141,0.443083840827794));
#16358=CARTESIAN_POINT('Ctrl Pts',(2.07802325244665,-5.70016260858665,0.558643359444972));
#16359=CARTESIAN_POINT('Ctrl Pts',(2.04454067222171,-5.71065575047077,0.672255788683429));
#16360=CARTESIAN_POINT('Ctrl Pts',(2.00193664484768,-5.72114886521972,0.782360480362788));
#16361=CARTESIAN_POINT('Ctrl Pts',(1.98421583250369,-5.72551339432251,0.828157666678365));
#16362=CARTESIAN_POINT('Ctrl Pts',(1.96491642180674,-5.7298779187307,0.873347683152784));
#16363=CARTESIAN_POINT('Ctrl Pts',(1.94404948782929,-5.73424243707816,0.917816577806229));
#16364=CARTESIAN_POINT('Ctrl Pts',(1.92410941887966,-5.73841309276118,0.960310258308687));
#16365=CARTESIAN_POINT('Ctrl Pts',(1.90274644225908,-5.74258374412136,1.00212694042875));
#16366=CARTESIAN_POINT('Ctrl Pts',(1.87997738447089,-5.74675439392095,1.04316107770339));
#16367=CARTESIAN_POINT('Ctrl Pts',(1.81856096074179,-5.75800415215426,1.15384505881766));
#16368=CARTESIAN_POINT('Ctrl Pts',(1.74691152655741,-5.76925389903309,1.25883281240855));
#16369=CARTESIAN_POINT('Ctrl Pts',(1.66663796485726,-5.78050368876758,1.35676769980135));
#16370=CARTESIAN_POINT('Ctrl Pts',(1.59359777283289,-5.79073977129635,1.44587777327455));
#16371=CARTESIAN_POINT('Ctrl Pts',(1.51341887038642,-5.80097588930537,1.52914854881905));
#16372=CARTESIAN_POINT('Ctrl Pts',(1.42733367458171,-5.8112120836312,1.60558955286148));
#16373=CARTESIAN_POINT('Ctrl Pts',(1.29936716837099,-5.82642828907195,1.71921987137455));
#16374=CARTESIAN_POINT('Ctrl Pts',(1.15800801595529,-5.84164433594918,1.81806817825947));
#16375=CARTESIAN_POINT('Ctrl Pts',(1.00701260070832,-5.8568603587367,1.89880465791413));
#16376=CARTESIAN_POINT('Ctrl Pts',(0.916140095555648,-5.86601771034833,
1.9473937236909));
#16377=CARTESIAN_POINT('Ctrl Pts',(0.821778444532971,-5.87517505323489,
1.98942241037955));
#16378=CARTESIAN_POINT('Ctrl Pts',(0.724754805610119,-5.88433241670825,
2.02416167134736));
#16379=CARTESIAN_POINT('Ctrl Pts',(0.711159816552476,-5.88561554994876,
2.02902934976029));
#16380=CARTESIAN_POINT('Ctrl Pts',(0.697512572004403,-5.88689868359346,
2.03375390628264));
#16381=CARTESIAN_POINT('Ctrl Pts',(0.683816070900821,-5.888181817723,2.03833533032528));
#16382=CARTESIAN_POINT('Ctrl Pts',(0.55685391361538,-5.9000760581528,2.08080365676094));
#16383=CARTESIAN_POINT('Ctrl Pts',(0.425875493423747,-5.91197028220641,
2.11090507367887));
#16384=CARTESIAN_POINT('Ctrl Pts',(0.293234341046548,-5.9238645247382,2.1287554216344));
#16385=CARTESIAN_POINT('Ctrl Pts',(0.152943045286072,-5.93644477352953,
2.14763529714494));
#16386=CARTESIAN_POINT('Ctrl Pts',(0.0107904063241632,-5.94902504299202,
2.15281057981495));
#16387=CARTESIAN_POINT('Ctrl Pts',(-0.13046881088098,-5.96160537436534,
2.14437022668701));
#16388=CARTESIAN_POINT('Ctrl Pts',(-0.143741864035601,-5.96278745232333,
2.14357715096475));
#16389=CARTESIAN_POINT('Ctrl Pts',(-0.157007040977092,-5.96396953082792,
2.14266382791756));
#16390=CARTESIAN_POINT('Ctrl Pts',(-0.170262062184394,-5.96515160991333,
2.14163030907934));
#16391=CARTESIAN_POINT('Ctrl Pts',(-0.280603216944505,-5.97499180324552,
2.1330268025069));
#16392=CARTESIAN_POINT('Ctrl Pts',(-0.390415974774632,-5.98483193806144,
2.11607611287816));
#16393=CARTESIAN_POINT('Ctrl Pts',(-0.498256555670661,-5.99467204205021,
2.09076297147814));
#16394=CARTESIAN_POINT('Ctrl Pts',(-0.597760479647373,-6.00375145307605,
2.06740667205402));
#16395=CARTESIAN_POINT('Ctrl Pts',(-0.695584319035439,-6.0128308378567,
2.036931429903));
#16396=CARTESIAN_POINT('Ctrl Pts',(-0.790595476208689,-6.02191021814334,
1.99936459740079));
#16397=CARTESIAN_POINT('Ctrl Pts',(-0.861094628275192,-6.02864720178338,
1.97148966232973));
#16398=CARTESIAN_POINT('Ctrl Pts',(-0.930045179462325,-6.03538418294912,
1.93971112476214));
#16399=CARTESIAN_POINT('Ctrl Pts',(-0.9971019628676,-6.04212117052666,1.90433818248478));
#16400=CARTESIAN_POINT('Ctrl Pts',(-1.09648359962445,-6.05210573611818,
1.85191364432608));
#16401=CARTESIAN_POINT('Ctrl Pts',(-1.19165717291185,-6.06209036860843,
1.79162701794501));
#16402=CARTESIAN_POINT('Ctrl Pts',(-1.28166486791139,-6.07207502071128,
1.72441933663095));
#16403=CARTESIAN_POINT('Ctrl Pts',(-1.37337957659669,-6.0822490337103,1.65593704838699));
#16404=CARTESIAN_POINT('Ctrl Pts',(-1.45973172270526,-6.09242306707288,
1.58026789185158));
#16405=CARTESIAN_POINT('Ctrl Pts',(-1.53968310678685,-6.10259707077108,
1.49836039146294));
#16406=CARTESIAN_POINT('Ctrl Pts',(-1.58288860032817,-6.10809507253954,
1.4540978184046));
#16407=CARTESIAN_POINT('Ctrl Pts',(-1.62422435978237,-6.11359306564514,
1.40801273570408));
#16408=CARTESIAN_POINT('Ctrl Pts',(-1.66352182264475,-6.1190910421929,1.36025057756247));
#16409=CARTESIAN_POINT('Ctrl Pts',(-1.72715791131522,-6.12799415444537,
1.28290724012521));
#16410=CARTESIAN_POINT('Ctrl Pts',(-1.78549671967051,-6.13689725176826,
1.20109991786849));
#16411=CARTESIAN_POINT('Ctrl Pts',(-1.83770840508035,-6.14580034330871,
1.11555659088419));
#16412=CARTESIAN_POINT('Ctrl Pts',(-1.86448675036628,-6.15036656363871,
1.0716831030067));
#16413=CARTESIAN_POINT('Ctrl Pts',(-1.88965392423985,-6.15493278244766,
1.0268275077978));
#16414=CARTESIAN_POINT('Ctrl Pts',(-1.91310209470199,-6.15949900096963,
0.981091420437047));
#16415=CARTESIAN_POINT('Ctrl Pts',(-1.95881902987313,-6.16840176447023,
0.891919698309309));
#16416=CARTESIAN_POINT('Ctrl Pts',(-1.99799829735294,-6.17730452687992,
0.799400097384168));
#16417=CARTESIAN_POINT('Ctrl Pts',(-2.03051224263836,-6.1862072973449,0.704628173813906));
#16418=CARTESIAN_POINT('Ctrl Pts',(-2.04250722654103,-6.18949169077914,
0.669665092967466));
#16419=CARTESIAN_POINT('Ctrl Pts',(-2.05359555039938,-6.1927760853097,0.634395617509192));
#16420=CARTESIAN_POINT('Ctrl Pts',(-2.06377255761049,-6.19606048139582,
0.598875080802976));
#16421=CARTESIAN_POINT('Ctrl Pts',(-2.09435351800118,-6.20592978624482,
0.492139170772034));
#16422=CARTESIAN_POINT('Ctrl Pts',(-2.11673115765934,-6.21579916446869,
0.383066308732467));
#16423=CARTESIAN_POINT('Ctrl Pts',(-2.13079348428194,-6.22566855405326,
0.272931722386978));
#16424=CARTESIAN_POINT('Ctrl Pts',(-2.14476120863747,-6.23547154874784,
0.163538050531035));
#16425=CARTESIAN_POINT('Ctrl Pts',(-2.15052521665063,-6.24527455465074,
0.0530955349082416));
#16426=CARTESIAN_POINT('Ctrl Pts',(-2.14792609857233,-6.25507751099098,
-0.0571533180216573));
#16427=CARTESIAN_POINT('Ctrl Pts',(-2.14633944053961,-6.26106182526724,
-0.12445585019977));
#16428=CARTESIAN_POINT('Ctrl Pts',(-2.14163519357573,-6.26704612107341,
-0.191686265490047));
#16429=CARTESIAN_POINT('Ctrl Pts',(-2.13376765524527,-6.2730303845844,-0.258559957831637));
#16430=CARTESIAN_POINT('Ctrl Pts',(-2.12322384350172,-6.28105029440031,
-0.348181843741631));
#16431=CARTESIAN_POINT('Ctrl Pts',(-2.10699630494181,-6.2890702054312,-0.437152810429182));
#16432=CARTESIAN_POINT('Ctrl Pts',(-2.0849960956876,-6.29709012135442,-0.524682076447492));
#16433=CARTESIAN_POINT('Ctrl Pts',(-2.05938271999409,-6.30642717434324,
-0.626586560573035));
#16434=CARTESIAN_POINT('Ctrl Pts',(-2.02594380632947,-6.31576423396336,
-0.726535670824349));
#16435=CARTESIAN_POINT('Ctrl Pts',(-1.98536504097984,-6.32510130601794,
-0.823502176291762));
#16436=CARTESIAN_POINT('Ctrl Pts',(-1.94929567093623,-6.33340077753115,
-0.909693087656475));
#16437=CARTESIAN_POINT('Ctrl Pts',(-1.90758625798322,-6.34170025886873,
-0.993527106597534));
#16438=CARTESIAN_POINT('Ctrl Pts',(-1.86074810235497,-6.34999975410607,
-1.07430040078544));
#16439=CARTESIAN_POINT('Ctrl Pts',(2.812123342995,-2.149914753478,-0.265823920622));
#16440=CARTESIAN_POINT('Ctrl Pts',(2.875955166892,-2.195775864589,0.4094462416164));
#16441=CARTESIAN_POINT('Ctrl Pts',(2.495432588024,-2.287498086811,1.80426843011));
#16442=CARTESIAN_POINT('Ctrl Pts',(0.6849378988389,-2.425081420145,3.00271269346));
#16443=CARTESIAN_POINT('Ctrl Pts',(-1.465969151843,-2.562664753478,2.708385870756));
#16444=CARTESIAN_POINT('Ctrl Pts',(-2.888423491095,-2.700248086811,1.068470223143));
#16445=CARTESIAN_POINT('Ctrl Pts',(-2.875636985226,-2.837831420145,-1.102416714848));
#16446=CARTESIAN_POINT('Ctrl Pts',(-1.433956868336,-2.975414753478,-2.725503141803));
#16447=CARTESIAN_POINT('Ctrl Pts',(0.7202502017102,-3.112998086811,-2.994301979619));
#16448=CARTESIAN_POINT('Ctrl Pts',(2.516567984095,-3.250581420145,-1.775243376929));
#16449=CARTESIAN_POINT('Ctrl Pts',(3.062413387288,-3.388164753478,0.32592613737));
#16450=CARTESIAN_POINT('Ctrl Pts',(2.086558092334,-3.525748086811,2.265144358043));
#16451=CARTESIAN_POINT('Ctrl Pts',(0.07390060109619,-3.663331420145,3.078821578666));
#16452=CARTESIAN_POINT('Ctrl Pts',(-1.975477796517,-3.800914753478,2.3626449362));
#16453=CARTESIAN_POINT('Ctrl Pts',(-3.043249345157,-3.938498086811,0.4724796727349));
#16454=CARTESIAN_POINT('Ctrl Pts',(-2.598842722989,-4.076081420145,-1.652458810098));
#16455=CARTESIAN_POINT('Ctrl Pts',(-0.8630817656259,-4.213664753478,-2.956297259047));
#16456=CARTESIAN_POINT('Ctrl Pts',(1.301540996194,-4.351248086811,-2.791163673665));
#16457=CARTESIAN_POINT('Ctrl Pts',(2.819433352591,-4.488831420145,-1.239112258151));
#16458=CARTESIAN_POINT('Ctrl Pts',(2.93636079082,-4.626414753478,0.928648977838));
#16459=CARTESIAN_POINT('Ctrl Pts',(1.594222544469,-4.763998086811,2.634968329346));
#16460=CARTESIAN_POINT('Ctrl Pts',(-0.5400783736277,-4.901581420145,3.031982679605));
#16461=CARTESIAN_POINT('Ctrl Pts',(-2.406016552425,-5.039164753478,1.922417218389));
#16462=CARTESIAN_POINT('Ctrl Pts',(-3.076414936985,-5.176748086811,-0.142389504376));
#16463=CARTESIAN_POINT('Ctrl Pts',(-2.218155287486,-5.314331420145,-2.136443475091));
#16464=CARTESIAN_POINT('Ctrl Pts',(-0.2577033950294,-5.451914753478,-3.068907366815));
#16465=CARTESIAN_POINT('Ctrl Pts',(1.830800486974,-5.589498086811,-2.476443876835));
#16466=CARTESIAN_POINT('Ctrl Pts',(3.009586244273,-5.727081420145,-0.653444959052));
#16467=CARTESIAN_POINT('Ctrl Pts',(2.69292402247,-5.864664753478,1.494245927945));
#16468=CARTESIAN_POINT('Ctrl Pts',(1.038147154526,-6.002248086811,2.899460185483));
#16469=CARTESIAN_POINT('Ctrl Pts',(-1.132437139127,-6.139831420145,2.863914402526));
#16470=CARTESIAN_POINT('Ctrl Pts',(-2.740480967886,-6.277414753478,1.405413643517));
#16471=CARTESIAN_POINT('Ctrl Pts',(-2.98618295317,-6.414998086811,-0.75185087581));
#16472=CARTESIAN_POINT('Ctrl Pts',(-2.162282365438,-6.506720309034,-1.939922503313));
#16473=CARTESIAN_POINT('Ctrl Pts',(-1.603965104547,-6.552581420145,-2.325079782801));
#16474=CARTESIAN_POINT('Ctrl Pts',(2.828248590073,-2.112003200128,-0.2673482052555));
#16475=CARTESIAN_POINT('Ctrl Pts',(2.89244643772,-2.157864311239,0.4117940838004));
#16476=CARTESIAN_POINT('Ctrl Pts',(2.50974187042,-2.249586533461,1.814614446512));
#16477=CARTESIAN_POINT('Ctrl Pts',(0.6888654622864,-2.387169866795,3.019930815918));
#16478=CARTESIAN_POINT('Ctrl Pts',(-1.474375296204,-2.524753200128,2.72391626755));
#16479=CARTESIAN_POINT('Ctrl Pts',(-2.904986257652,-2.662336533461,1.074597033472));
#16480=CARTESIAN_POINT('Ctrl Pts',(-2.892126431541,-2.799919866795,-1.10873818078));
#16481=CARTESIAN_POINT('Ctrl Pts',(-1.442179448209,-2.937503200128,-2.741131692266));
#16482=CARTESIAN_POINT('Ctrl Pts',(0.7243802525807,-3.075086533461,-3.011471873454));
#16483=CARTESIAN_POINT('Ctrl Pts',(2.53099846085,-3.212669866795,-1.785422958187));
#16484=CARTESIAN_POINT('Ctrl Pts',(3.079973844815,-3.350253200128,0.3277950594809));
#16485=CARTESIAN_POINT('Ctrl Pts',(2.098522811046,-3.487836533461,2.278133124177));
#16486=CARTESIAN_POINT('Ctrl Pts',(0.07432436111898,-3.625419866795,3.096476123865));
#16487=CARTESIAN_POINT('Ctrl Pts',(-1.986805559805,-3.763003200128,2.376192789088));
#16488=CARTESIAN_POINT('Ctrl Pts',(-3.060699912442,-3.900586533461,0.4751889605338));
#16489=CARTESIAN_POINT('Ctrl Pts',(-2.613744978657,-4.038169866795,-1.661934321428));
#16490=CARTESIAN_POINT('Ctrl Pts',(-0.8680308396962,-4.175753200128,-2.973249226626));
#16491=CARTESIAN_POINT('Ctrl Pts',(1.309004278414,-4.313336533461,-2.807168734035));
#16492=CARTESIAN_POINT('Ctrl Pts',(2.835600516647,-4.450919866795,-1.24621756218));
#16493=CARTESIAN_POINT('Ctrl Pts',(2.95319843892,-4.588503200128,0.9339740267032));
#16494=CARTESIAN_POINT('Ctrl Pts',(1.603364118038,-4.726086533461,2.650077736072));
#16495=CARTESIAN_POINT('Ctrl Pts',(-0.5431752851618,-4.863669866795,3.049368641699));
#16496=CARTESIAN_POINT('Ctrl Pts',(-2.419813106363,-5.001253200128,1.933440722287));
#16497=CARTESIAN_POINT('Ctrl Pts',(-3.094055682046,-5.138836533461,-0.1432059927228));
#16498=CARTESIAN_POINT('Ctrl Pts',(-2.230874609403,-5.276419866795,-2.148694246022));
#16499=CARTESIAN_POINT('Ctrl Pts',(-0.2591811150334,-5.414003200128,-3.086505062049));
#16500=CARTESIAN_POINT('Ctrl Pts',(1.841298643208,-5.551586533461,-2.49064427437));
#16501=CARTESIAN_POINT('Ctrl Pts',(3.026843780971,-5.689169866795,-0.6571919360268));
#16502=CARTESIAN_POINT('Ctrl Pts',(2.708365758102,-5.826753200128,1.502814216688));
#16503=CARTESIAN_POINT('Ctrl Pts',(1.044100086645,-5.964336533461,2.916086238533));
#16504=CARTESIAN_POINT('Ctrl Pts',(-1.13893074785,-6.101919866795,2.880336629334));
#16505=CARTESIAN_POINT('Ctrl Pts',(-2.756195404036,-6.239503200128,1.413472551141));
#16506=CARTESIAN_POINT('Ctrl Pts',(-3.003306290972,-6.377086533461,-0.7561621309221));
#16507=CARTESIAN_POINT('Ctrl Pts',(-2.174681301453,-6.468808755684,-1.951046385826));
#16508=CARTESIAN_POINT('Ctrl Pts',(-1.613162543799,-6.514669866795,-2.338412229995));
#16509=CARTESIAN_POINT('Ctrl Pts',(2.877175670666,-1.897001600064,-0.2719731760698));
#16510=CARTESIAN_POINT('Ctrl Pts',(2.942484104304,-1.942862711175,0.4189178855753));
#16511=CARTESIAN_POINT('Ctrl Pts',(2.553158967202,-2.034584933397,1.846006237029));
#16512=CARTESIAN_POINT('Ctrl Pts',(0.700782440203,-2.172168266731,3.072173889222));
#16513=CARTESIAN_POINT('Ctrl Pts',(-1.499881144309,-2.309751600064,2.771038458724));
#16514=CARTESIAN_POINT('Ctrl Pts',(-2.955240855938,-2.447334933397,1.093186946624));
#16515=CARTESIAN_POINT('Ctrl Pts',(-2.942158562201,-2.584918266731,-1.127918716224));
#16516=CARTESIAN_POINT('Ctrl Pts',(-1.467128326585,-2.722501600064,-2.788551700427));
#16517=CARTESIAN_POINT('Ctrl Pts',(0.7369116160266,-2.860084933397,-3.063568611899));
#16518=CARTESIAN_POINT('Ctrl Pts',(2.574783284471,-2.997668266731,-1.816309752677));
#16519=CARTESIAN_POINT('Ctrl Pts',(3.133255628127,-3.135251600064,0.3334657262495));
#16520=CARTESIAN_POINT('Ctrl Pts',(2.134826053647,-3.272834933397,2.317543522314));
#16521=CARTESIAN_POINT('Ctrl Pts',(0.07561012999347,-3.410418266731,3.150043387152));
#16522=CARTESIAN_POINT('Ctrl Pts',(-2.02117615795,-3.548001600064,2.41729956326));
#16523=CARTESIAN_POINT('Ctrl Pts',(-3.113648267764,-3.685584933397,0.4834094573636));
#16524=CARTESIAN_POINT('Ctrl Pts',(-2.658961269639,-3.823168266731,-1.690684833236));
#16525=CARTESIAN_POINT('Ctrl Pts',(-0.8830472760164,-3.960751600064,-3.024684735174));
#16526=CARTESIAN_POINT('Ctrl Pts',(1.331649302635,-4.098334933397,-2.855731145192));
#16527=CARTESIAN_POINT('Ctrl Pts',(2.884654781358,-4.235918266731,-1.267776412174));
#16528=CARTESIAN_POINT('Ctrl Pts',(3.004287080326,-4.373501600064,0.9501312423865));
#16529=CARTESIAN_POINT('Ctrl Pts',(1.631101398876,-4.511084933397,2.695922562946));
#16530=CARTESIAN_POINT('Ctrl Pts',(-0.5525719064653,-4.648668266731,3.102120972527));
#16531=CARTESIAN_POINT('Ctrl Pts',(-2.461674487038,-4.786251600064,1.966888139311));
#16532=CARTESIAN_POINT('Ctrl Pts',(-3.147581073076,-4.923834933397,-0.1456833743688));
#16533=CARTESIAN_POINT('Ctrl Pts',(-2.269467462304,-5.061418266731,-2.185865425709));
#16534=CARTESIAN_POINT('Ctrl Pts',(-0.263664799865,-5.199001600064,-3.139899831678));
#16535=CARTESIAN_POINT('Ctrl Pts',(1.873152055043,-5.336584933397,-2.53373099368));
#16536=CARTESIAN_POINT('Ctrl Pts',(3.079206444611,-5.474168266731,-0.6685609800817));
#16537=CARTESIAN_POINT('Ctrl Pts',(2.755218934369,-5.611751600064,1.528812041827));
#16538=CARTESIAN_POINT('Ctrl Pts',(1.062162420085,-5.749334933397,2.966532860131));
#16539=CARTESIAN_POINT('Ctrl Pts',(-1.15863359741,-5.886918266731,2.930164803169));
#16540=CARTESIAN_POINT('Ctrl Pts',(-2.803876005782,-6.024501600064,1.437924816642));
#16541=CARTESIAN_POINT('Ctrl Pts',(-3.055261769517,-6.162084933397,-0.7692433026587));
#16542=CARTESIAN_POINT('Ctrl Pts',(-2.212302042314,-6.25380715562,-1.984798370744));
#16543=CARTESIAN_POINT('Ctrl Pts',(-1.64106933179,-6.299668266731,-2.378865422135));
#16544=CARTESIAN_POINT('Ctrl Pts',(2.488904911508,-1.507,-0.2352707832963));
#16545=CARTESIAN_POINT('Ctrl Pts',(2.545400065037,-1.552861111111,0.3623855135288));
#16546=CARTESIAN_POINT('Ctrl Pts',(2.208613800721,-1.644583333333,1.596890324375));
#16547=CARTESIAN_POINT('Ctrl Pts',(0.6062128479337,-1.782166666667,2.657588398181));
#16548=CARTESIAN_POINT('Ctrl Pts',(-1.297474319976,-1.91975,2.397090765159));
#16549=CARTESIAN_POINT('Ctrl Pts',(-2.556435311206,-2.057333333333,0.9456629250653));
#16550=CARTESIAN_POINT('Ctrl Pts',(-2.545118454378,-2.194916666667,-0.9757076918219));
#16551=CARTESIAN_POINT('Ctrl Pts',(-1.269141448358,-2.3325,-2.412240619837));
#16552=CARTESIAN_POINT('Ctrl Pts',(0.6374664429341,-2.470083333333,-2.650144390777));
#16553=CARTESIAN_POINT('Ctrl Pts',(2.22731994717,-2.607666666667,-1.571201338294));
#16554=CARTESIAN_POINT('Ctrl Pts',(2.710427243412,-2.74525,0.2884650014053));
#16555=CARTESIAN_POINT('Ctrl Pts',(1.846734318071,-2.882833333333,2.004794324563));
#16556=CARTESIAN_POINT('Ctrl Pts',(0.06540665063282,-3.020416666667,2.724949518265));
#16557=CARTESIAN_POINT('Ctrl Pts',(-1.748421313941,-3.158,2.091088429853));
#16558=CARTESIAN_POINT('Ctrl Pts',(-2.693465868406,-3.295583333333,0.4181740395515));
#16559=CARTESIAN_POINT('Ctrl Pts',(-2.300138233124,-3.433166666667,-1.46252932282));
#16560=CARTESIAN_POINT('Ctrl Pts',(-0.7638813037308,-3.57075,-2.616507837839));
#16561=CARTESIAN_POINT('Ctrl Pts',(1.151945125744,-3.708333333333,-2.470354294206));
#16562=CARTESIAN_POINT('Ctrl Pts',(2.495374726863,-3.845916666667,-1.096691790885));
#16563=CARTESIAN_POINT('Ctrl Pts',(2.598862817463,-3.9835,0.8219123843785));
#16564=CARTESIAN_POINT('Ctrl Pts',(1.41098658807,-4.121083333333,2.332111652539));
#16565=CARTESIAN_POINT('Ctrl Pts',(-0.4780031146462,-4.258666666667,2.683494165244));
#16566=CARTESIAN_POINT('Ctrl Pts',(-2.129475020865,-4.39625,1.701459386102));
#16567=CARTESIAN_POINT('Ctrl Pts',(-2.722819489967,-4.533833333333,-0.1260236104762));
#16568=CARTESIAN_POINT('Ctrl Pts',(-1.963206060383,-4.671416666667,-1.890885999562));
#16569=CARTESIAN_POINT('Ctrl Pts',(-0.2280836106277,-4.809,-2.716174821156));
#16570=CARTESIAN_POINT('Ctrl Pts',(1.620372852909,-4.946583333333,-2.191807604556));
#16571=CARTESIAN_POINT('Ctrl Pts',(2.663671920236,-5.084166666667,-0.5783396279667));
#16572=CARTESIAN_POINT('Ctrl Pts',(2.383406063087,-5.22175,1.322501034076));
#16573=CARTESIAN_POINT('Ctrl Pts',(0.9188251141986,-5.359333333333,2.566203475515));
#16574=CARTESIAN_POINT('Ctrl Pts',(-1.002277643535,-5.496916666667,2.534743236046));
#16575=CARTESIAN_POINT('Ctrl Pts',(-2.425496932009,-5.6345,1.243878910491));
#16576=CARTESIAN_POINT('Ctrl Pts',(-2.642958544944,-5.772083333333,-0.6654350145011));
#16577=CARTESIAN_POINT('Ctrl Pts',(-1.913755032407,-5.863805555556,-1.71695265731));
#16578=CARTESIAN_POINT('Ctrl Pts',(-1.419609362633,-5.909666666667,-2.057840921336));
#16579=CARTESIAN_POINT('Ctrl Pts',(2.10063415235,-1.897001600064,-0.1985683905227));
#16580=CARTESIAN_POINT('Ctrl Pts',(2.14831602577,-1.942862711175,0.3058531414823));
#16581=CARTESIAN_POINT('Ctrl Pts',(1.864068634239,-2.034584933397,1.347774411722));
#16582=CARTESIAN_POINT('Ctrl Pts',(0.5116432556643,-2.172168266731,2.24300290714));
#16583=CARTESIAN_POINT('Ctrl Pts',(-1.095067495643,-2.309751600064,2.023143071595));
#16584=CARTESIAN_POINT('Ctrl Pts',(-2.157629766474,-2.447334933397,0.7981389035067));
#16585=CARTESIAN_POINT('Ctrl Pts',(-2.148078346554,-2.584918266731,-0.8234966674198));
#16586=CARTESIAN_POINT('Ctrl Pts',(-1.071154570131,-2.722501600064,-2.035929539246));
#16587=CARTESIAN_POINT('Ctrl Pts',(0.5380212698415,-2.860084933397,-2.236720169656));
#16588=CARTESIAN_POINT('Ctrl Pts',(1.87985660987,-2.997668266731,-1.326092923911));
#16589=CARTESIAN_POINT('Ctrl Pts',(2.287598858697,-3.135251600064,0.2434642765611));
#16590=CARTESIAN_POINT('Ctrl Pts',(1.558642582494,-3.272834933397,1.692045126811));
#16591=CARTESIAN_POINT('Ctrl Pts',(0.05520317127216,-3.410418266731,2.299855649378));
#16592=CARTESIAN_POINT('Ctrl Pts',(-1.475666469932,-3.548001600064,1.764877296446));
#16593=CARTESIAN_POINT('Ctrl Pts',(-2.273283469047,-3.685584933397,0.3529386217393));
#16594=CARTESIAN_POINT('Ctrl Pts',(-1.941315196609,-3.823168266731,-1.234373812404));
#16595=CARTESIAN_POINT('Ctrl Pts',(-0.6447153314452,-3.960751600064,-2.208330940504));
#16596=CARTESIAN_POINT('Ctrl Pts',(0.972240948854,-4.098334933397,-2.08497744322));
#16597=CARTESIAN_POINT('Ctrl Pts',(2.106094672369,-4.235918266731,-0.9256071695965));
#16598=CARTESIAN_POINT('Ctrl Pts',(2.1934385546,-4.373501600064,0.6936935263705));
#16599=CARTESIAN_POINT('Ctrl Pts',(1.190871777263,-4.511084933397,1.968300742132));
#16600=CARTESIAN_POINT('Ctrl Pts',(-0.4034343228272,-4.648668266731,2.264867357961));
#16601=CARTESIAN_POINT('Ctrl Pts',(-1.797275554691,-4.786251600064,1.436030632892));
#16602=CARTESIAN_POINT('Ctrl Pts',(-2.298057906858,-4.923834933397,-0.1063638465836));
#16603=CARTESIAN_POINT('Ctrl Pts',(-1.656944658461,-5.061418266731,-1.595906573415));
#16604=CARTESIAN_POINT('Ctrl Pts',(-0.1925024213904,-5.199001600064,-2.292449810634));
#16605=CARTESIAN_POINT('Ctrl Pts',(1.367593650775,-5.336584933397,-1.849884215432));
#16606=CARTESIAN_POINT('Ctrl Pts',(2.248137395861,-5.474168266731,-0.4881182758517));
#16607=CARTESIAN_POINT('Ctrl Pts',(2.011593191805,-5.611751600064,1.116190026326));
#16608=CARTESIAN_POINT('Ctrl Pts',(0.775487808312,-5.749334933397,2.165874090898));
#16609=CARTESIAN_POINT('Ctrl Pts',(-0.8459216896603,-5.886918266731,2.139321668922));
#16610=CARTESIAN_POINT('Ctrl Pts',(-2.047117858235,-6.024501600064,1.04983300434));
#16611=CARTESIAN_POINT('Ctrl Pts',(-2.230655320372,-6.162084933397,-0.5616267263435));
#16612=CARTESIAN_POINT('Ctrl Pts',(-1.615208022499,-6.25380715562,-1.449106943876));
#16613=CARTESIAN_POINT('Ctrl Pts',(-1.198149393476,-6.299668266731,-1.736816420537));
#16614=CARTESIAN_POINT('Ctrl Pts',(2.149561232942,-2.112003200128,-0.2031933613371));
#16615=CARTESIAN_POINT('Ctrl Pts',(2.198353692354,-2.157864311239,0.3129769432571));
#16616=CARTESIAN_POINT('Ctrl Pts',(1.907485731021,-2.249586533461,1.379166202239));
#16617=CARTESIAN_POINT('Ctrl Pts',(0.5235602335809,-2.387169866795,2.295245980444));
#16618=CARTESIAN_POINT('Ctrl Pts',(-1.120573343748,-2.524753200128,2.070265262769));
#16619=CARTESIAN_POINT('Ctrl Pts',(-2.20788436476,-2.662336533461,0.8167288166584));
#16620=CARTESIAN_POINT('Ctrl Pts',(-2.198110477214,-2.799919866795,-0.842677202864));
#16621=CARTESIAN_POINT('Ctrl Pts',(-1.096103448508,-2.937503200128,-2.083349547407));
#16622=CARTESIAN_POINT('Ctrl Pts',(0.5505526332874,-3.075086533461,-2.2888169081));
#16623=CARTESIAN_POINT('Ctrl Pts',(1.923641433491,-3.212669866795,-1.3569797184));
#16624=CARTESIAN_POINT('Ctrl Pts',(2.340880642008,-3.350253200128,0.2491349433296));
#16625=CARTESIAN_POINT('Ctrl Pts',(1.594945825095,-3.487836533461,1.731455524949));
#16626=CARTESIAN_POINT('Ctrl Pts',(0.05648894014665,-3.625419866795,2.353422912665));
#16627=CARTESIAN_POINT('Ctrl Pts',(-1.510037068078,-3.763003200128,1.805984070618));
#16628=CARTESIAN_POINT('Ctrl Pts',(-2.326231824369,-3.900586533461,0.3611591185692));
#16629=CARTESIAN_POINT('Ctrl Pts',(-1.986531487591,-4.038169866795,-1.263124324211));
#16630=CARTESIAN_POINT('Ctrl Pts',(-0.6597317677653,-4.175753200128,-2.259766449053));
#16631=CARTESIAN_POINT('Ctrl Pts',(0.9948859730751,-4.313336533461,-2.133539854377));
#16632=CARTESIAN_POINT('Ctrl Pts',(2.15514893708,-4.450919866795,-0.9471660195909));
#16633=CARTESIAN_POINT('Ctrl Pts',(2.244527196006,-4.588503200128,0.7098507420537));
#16634=CARTESIAN_POINT('Ctrl Pts',(1.218609058101,-4.726086533461,2.014145569006));
#16635=CARTESIAN_POINT('Ctrl Pts',(-0.4128309441306,-4.863669866795,2.317619688789));
#16636=CARTESIAN_POINT('Ctrl Pts',(-1.839136935367,-5.001253200128,1.469478049916));
#16637=CARTESIAN_POINT('Ctrl Pts',(-2.351583297887,-5.138836533461,-0.1088412282295));
#16638=CARTESIAN_POINT('Ctrl Pts',(-1.695537511362,-5.276419866795,-1.633077753103));
#16639=CARTESIAN_POINT('Ctrl Pts',(-0.196986106222,-5.414003200128,-2.345844580263));
#16640=CARTESIAN_POINT('Ctrl Pts',(1.39944706261,-5.551586533461,-1.892970934742));
#16641=CARTESIAN_POINT('Ctrl Pts',(2.300500059501,-5.689169866795,-0.4994873199066));
#16642=CARTESIAN_POINT('Ctrl Pts',(2.058446368072,-5.826753200128,1.142187851465));
#16643=CARTESIAN_POINT('Ctrl Pts',(0.7935501417522,-5.964336533461,2.216320712496));
#16644=CARTESIAN_POINT('Ctrl Pts',(-0.8656245392205,-6.101919866795,2.189149842758));
#16645=CARTESIAN_POINT('Ctrl Pts',(-2.094798459981,-6.239503200128,1.07428526984));
#16646=CARTESIAN_POINT('Ctrl Pts',(-2.282610798917,-6.377086533461,-0.5747078980801));
#16647=CARTESIAN_POINT('Ctrl Pts',(-1.652828763361,-6.468808755684,-1.482858928795));
#16648=CARTESIAN_POINT('Ctrl Pts',(-1.226056181467,-6.514669866795,-1.777269612677));
#16649=CARTESIAN_POINT('Ctrl Pts',(2.16568648002,-2.149914753478,-0.2047176459706));
#16650=CARTESIAN_POINT('Ctrl Pts',(2.214844963183,-2.195775864589,0.3153247854411));
#16651=CARTESIAN_POINT('Ctrl Pts',(1.921795013418,-2.287498086811,1.389512218641));
#16652=CARTESIAN_POINT('Ctrl Pts',(0.5274877970284,-2.425081420145,2.312464102902));
#16653=CARTESIAN_POINT('Ctrl Pts',(-1.128979488109,-2.562664753478,2.085795659563));
#16654=CARTESIAN_POINT('Ctrl Pts',(-2.224447131318,-2.700248086811,0.8228556269872));
#16655=CARTESIAN_POINT('Ctrl Pts',(-2.214599923529,-2.837831420145,-0.8489986687962));
#16656=CARTESIAN_POINT('Ctrl Pts',(-1.104326028381,-2.975414753478,-2.09897809787));
#16657=CARTESIAN_POINT('Ctrl Pts',(0.5546826841579,-3.112998086811,-2.305986801935));
#16658=CARTESIAN_POINT('Ctrl Pts',(1.938071910246,-3.250581420145,-1.367159299658));
#16659=CARTESIAN_POINT('Ctrl Pts',(2.358441099535,-3.388164753478,0.2510038654405));
#16660=CARTESIAN_POINT('Ctrl Pts',(1.606910543807,-3.525748086811,1.744444291083));
#16661=CARTESIAN_POINT('Ctrl Pts',(0.05691270016944,-3.663331420145,2.371077457865));
#16662=CARTESIAN_POINT('Ctrl Pts',(-1.521364831366,-3.800914753478,1.819531923506));
#16663=CARTESIAN_POINT('Ctrl Pts',(-2.343682391654,-3.938498086811,0.3638684063681));
#16664=CARTESIAN_POINT('Ctrl Pts',(-2.001433743259,-4.076081420145,-1.272599835542));
#16665=CARTESIAN_POINT('Ctrl Pts',(-0.6646808418357,-4.213664753478,-2.276718416632));
#16666=CARTESIAN_POINT('Ctrl Pts',(1.002349255295,-4.351248086811,-2.149544914748));
#16667=CARTESIAN_POINT('Ctrl Pts',(2.171316101136,-4.488831420145,-0.9542713236204));
#16668=CARTESIAN_POINT('Ctrl Pts',(2.261364844106,-4.626414753478,0.715175790919));
#16669=CARTESIAN_POINT('Ctrl Pts',(1.227750631671,-4.763998086811,2.029254975732));
#16670=CARTESIAN_POINT('Ctrl Pts',(-0.4159278556647,-4.901581420145,2.335005650883));
#16671=CARTESIAN_POINT('Ctrl Pts',(-1.852933489305,-5.039164753478,1.480501553815));
#16672=CARTESIAN_POINT('Ctrl Pts',(-2.369224042948,-5.176748086811,-0.1096577165763));
#16673=CARTESIAN_POINT('Ctrl Pts',(-1.708256833279,-5.314331420145,-1.645328524034));
#16674=CARTESIAN_POINT('Ctrl Pts',(-0.198463826226,-5.451914753478,-2.363442275497));
#16675=CARTESIAN_POINT('Ctrl Pts',(1.409945218843,-5.589498086811,-1.907171332278));
#16676=CARTESIAN_POINT('Ctrl Pts',(2.317757596199,-5.727081420145,-0.5032342968815));
#16677=CARTESIAN_POINT('Ctrl Pts',(2.073888103704,-5.864664753478,1.150756140208));
#16678=CARTESIAN_POINT('Ctrl Pts',(0.7995030738709,-6.002248086811,2.232946765546));
#16679=CARTESIAN_POINT('Ctrl Pts',(-0.872118147943,-6.139831420145,2.205572069566));
#16680=CARTESIAN_POINT('Ctrl Pts',(-2.110512896131,-6.277414753478,1.082344177464));
#16681=CARTESIAN_POINT('Ctrl Pts',(-2.299734136718,-6.414998086811,-0.5790191531922));
#16682=CARTESIAN_POINT('Ctrl Pts',(-1.665227699375,-6.506720309034,-1.493982811308));
#16683=CARTESIAN_POINT('Ctrl Pts',(-1.235253620718,-6.552581420145,-1.790602059871));
#16684=CARTESIAN_POINT('Ctrl Pts',(-2.46657132033207,-6.35000032196148,
-1.42407561576919));
#16685=CARTESIAN_POINT('Ctrl Pts',(-2.46656773371528,-6.32633902069027,
-1.42407354503503));
#16686=CARTESIAN_POINT('Ctrl Pts',(-2.46379616437334,-6.30282232723362,
-1.42247337872942));
#16687=CARTESIAN_POINT('Ctrl Pts',(-2.45356483291024,-6.25653765529766,
-1.41656631675503));
#16688=CARTESIAN_POINT('Ctrl Pts',(-2.44603863170313,-6.2338753697584,-1.41222106246213));
#16689=CARTESIAN_POINT('Ctrl Pts',(-2.41606465188457,-6.16483033080454,
-1.39491557714521));
#16690=CARTESIAN_POINT('Ctrl Pts',(-2.38620330258456,-6.12184666366958,
-1.37767511908847));
#16691=CARTESIAN_POINT('Ctrl Pts',(-2.32200501666487,-6.0584711962758,-1.34061022143123));
#16692=CARTESIAN_POINT('Ctrl Pts',(-2.28848517345059,-6.0347538130208,-1.32125753092827));
#16693=CARTESIAN_POINT('Ctrl Pts',(-2.2245246425145,-6.00727203284357,-1.2843299011748));
#16694=CARTESIAN_POINT('Ctrl Pts',(-2.19496853427892,-6.00026455306915,
-1.26726567412879));
#16695=CARTESIAN_POINT('Ctrl Pts',(-2.13510893685025,-5.999837714383,-1.23270571943976));
#16696=CARTESIAN_POINT('Ctrl Pts',(-2.10551526912305,-6.00648534402824,
-1.21561980741115));
#16697=CARTESIAN_POINT('Ctrl Pts',(-2.04167439680108,-6.03308499838888,
-1.17876126259076));
#16698=CARTESIAN_POINT('Ctrl Pts',(-2.00822262138601,-6.0562371212313,-1.15944787105));
#16699=CARTESIAN_POINT('Ctrl Pts',(-1.94373392235482,-6.11855684463581,
-1.12221530330465));
#16700=CARTESIAN_POINT('Ctrl Pts',(-1.91354181190603,-6.16110729445364,
-1.10478388020964));
#16701=CARTESIAN_POINT('Ctrl Pts',(-1.88254279196225,-6.23033336303122,
-1.08688658770048));
#16702=CARTESIAN_POINT('Ctrl Pts',(-1.87455993512035,-6.25365009437143,
-1.08227768315391));
#16703=CARTESIAN_POINT('Ctrl Pts',(-1.863700740893,-6.30133148665094,-1.07600812444357));
#16704=CARTESIAN_POINT('Ctrl Pts',(-1.86075053790222,-6.32558725065952,
-1.07430482395264));
#16705=CARTESIAN_POINT('Ctrl Pts',(-1.86074679171387,-6.34999975408563,
-1.07430266108979));
#16706=CARTESIAN_POINT('Origin',(-2.165063509461,-6.35,-1.25));
#16707=CARTESIAN_POINT('',(0.,0.,0.));
#16708=CARTESIAN_POINT('Origin',(0.,0.,0.));
#16709=CARTESIAN_POINT('',(-2.,-3.464101615138,0.));
#16710=CARTESIAN_POINT('',(2.,-3.464101615138,0.));
#16711=CARTESIAN_POINT('',(-2.,-3.464101615138,0.));
#16712=CARTESIAN_POINT('',(-4.,0.,0.));
#16713=CARTESIAN_POINT('',(-4.,0.,0.));
#16714=CARTESIAN_POINT('',(-2.,3.464101615138,0.));
#16715=CARTESIAN_POINT('',(-2.,3.464101615138,0.));
#16716=CARTESIAN_POINT('',(2.,3.464101615138,0.));
#16717=CARTESIAN_POINT('',(2.,3.464101615138,0.));
#16718=CARTESIAN_POINT('',(4.,0.,0.));
#16719=CARTESIAN_POINT('',(4.,0.,0.));
#16720=CARTESIAN_POINT('',(2.,-3.464101615138,0.));
#16721=CARTESIAN_POINT('',(-1.75,-2.14313189850787E-16,0.));
#16722=CARTESIAN_POINT('Origin',(0.,0.,0.));
#16723=CARTESIAN_POINT('Origin',(0.,0.,0.));
#16724=CARTESIAN_POINT('',(-1.75,-2.14313189850787E-16,4.));
#16725=CARTESIAN_POINT('',(-1.75,-2.14313189850787E-16,0.));
#16726=CARTESIAN_POINT('Origin',(0.,0.,4.));
#16727=CARTESIAN_POINT('Origin',(0.,0.,4.));
#16728=CARTESIAN_POINT('',(-2.,-3.464101615138,4.));
#16729=CARTESIAN_POINT('',(2.,-3.464101615138,4.));
#16730=CARTESIAN_POINT('',(-2.,-3.464101615138,4.));
#16731=CARTESIAN_POINT('',(4.,0.,4.));
#16732=CARTESIAN_POINT('',(2.,-3.464101615138,4.));
#16733=CARTESIAN_POINT('',(2.,3.464101615138,4.));
#16734=CARTESIAN_POINT('',(4.,0.,4.));
#16735=CARTESIAN_POINT('',(-2.,3.464101615138,4.));
#16736=CARTESIAN_POINT('',(2.,3.464101615138,4.));
#16737=CARTESIAN_POINT('',(-4.,0.,4.));
#16738=CARTESIAN_POINT('',(-2.,3.464101615138,4.));
#16739=CARTESIAN_POINT('',(-4.,0.,4.));
#16740=CARTESIAN_POINT('Origin',(-2.,-3.464101615138,0.));
#16741=CARTESIAN_POINT('',(2.,-3.464101615138,0.));
#16742=CARTESIAN_POINT('',(-2.,-3.464101615138,0.));
#16743=CARTESIAN_POINT('Origin',(-4.,0.,0.));
#16744=CARTESIAN_POINT('',(-4.,0.,0.));
#16745=CARTESIAN_POINT('Origin',(-2.,3.464101615138,0.));
#16746=CARTESIAN_POINT('',(-2.,3.464101615138,0.));
#16747=CARTESIAN_POINT('Origin',(2.,3.464101615138,0.));
#16748=CARTESIAN_POINT('',(2.,3.464101615138,0.));
#16749=CARTESIAN_POINT('Origin',(4.,0.,0.));
#16750=CARTESIAN_POINT('',(4.,0.,0.));
#16751=CARTESIAN_POINT('Origin',(2.,-3.464101615138,0.));
#16752=CARTESIAN_POINT('Origin',(0.,0.,4.));
#16753=CARTESIAN_POINT('',(-2.,-2.44929359829471E-16,4.));
#16754=CARTESIAN_POINT('Origin',(0.,0.,4.));
#16755=CARTESIAN_POINT('',(-2.,-2.44929359829471E-16,0.));
#16756=CARTESIAN_POINT('',(-2.,-2.44929359829471E-16,4.));
#16757=CARTESIAN_POINT('Origin',(0.,0.,0.));
#16758=CARTESIAN_POINT('Origin',(0.,0.,0.));
#16759=CARTESIAN_POINT('',(1.75,0.,0.));
#16760=CARTESIAN_POINT('Origin',(0.,0.,0.));
#16761=CARTESIAN_POINT('',(0.,0.,0.));
#16762=CARTESIAN_POINT('',(0.,0.,0.));
#16763=CARTESIAN_POINT('Origin',(0.,0.,0.));
#16764=CARTESIAN_POINT('',(3.162277660168,0.,3.5));
#16765=CARTESIAN_POINT('',(4.969293465979,0.,2.357142857143));
#16766=CARTESIAN_POINT('Origin',(3.162277660168,0.,1.5));
#16767=CARTESIAN_POINT('',(4.969293465979,0.,-2.357142857143));
#16768=CARTESIAN_POINT('Origin',(0.,0.,0.));
#16769=CARTESIAN_POINT('',(3.162277660168,0.,-3.5));
#16770=CARTESIAN_POINT('Origin',(3.162277660168,0.,-1.5));
#16771=CARTESIAN_POINT('',(-3.162277660168,0.,-3.5));
#16772=CARTESIAN_POINT('',(3.162277660168,0.,-3.5));
#16773=CARTESIAN_POINT('',(-4.969293465979,0.,-2.357142857143));
#16774=CARTESIAN_POINT('Origin',(-3.162277660168,0.,-1.5));
#16775=CARTESIAN_POINT('',(-4.969293465979,0.,2.357142857143));
#16776=CARTESIAN_POINT('Origin',(0.,0.,0.));
#16777=CARTESIAN_POINT('',(-3.162277660168,0.,3.5));
#16778=CARTESIAN_POINT('Origin',(-3.162277660168,0.,1.5));
#16779=CARTESIAN_POINT('',(-3.162277660168,0.,3.5));
#16780=CARTESIAN_POINT('Origin',(3.162277660168,24.7684,1.5));
#16781=CARTESIAN_POINT('',(4.969293465979,-13.,2.357142857143));
#16782=CARTESIAN_POINT('',(3.162277660168,-13.,3.5));
#16783=CARTESIAN_POINT('Origin',(3.162277660168,-13.,1.5));
#16784=CARTESIAN_POINT('',(4.969293465979,0.,2.357142857143));
#16785=CARTESIAN_POINT('',(3.162277660168,0.,3.5));
#16786=CARTESIAN_POINT('Origin',(0.,-13.,0.));
#16787=CARTESIAN_POINT('',(-2.14313189850787E-16,-13.,1.75));
#16788=CARTESIAN_POINT('Origin',(0.,-13.,0.));
#16789=CARTESIAN_POINT('Origin',(0.,-13.,0.));
#16790=CARTESIAN_POINT('',(2.828427124746,-13.,3.5));
#16791=CARTESIAN_POINT('',(-2.1213203435595,-13.,3.5));
#16792=CARTESIAN_POINT('',(2.828427124746,-13.,-3.5));
#16793=CARTESIAN_POINT('Origin',(0.,-13.,0.));
#16794=CARTESIAN_POINT('',(3.162277660168,-13.,-3.5));
#16795=CARTESIAN_POINT('',(2.1213203435595,-13.,-3.5));
#16796=CARTESIAN_POINT('',(4.969293465979,-13.,-2.357142857143));
#16797=CARTESIAN_POINT('Origin',(3.162277660168,-13.,-1.5));
#16798=CARTESIAN_POINT('Origin',(0.,-13.,0.));
#16799=CARTESIAN_POINT('Origin',(0.,-13.,0.));
#16800=CARTESIAN_POINT('',(-4.969293465979,-13.,-2.357142857143));
#16801=CARTESIAN_POINT('',(-3.162277660168,-13.,-3.5));
#16802=CARTESIAN_POINT('Origin',(-3.162277660168,-13.,-1.5));
#16803=CARTESIAN_POINT('',(-2.828427124746,-13.,-3.5));
#16804=CARTESIAN_POINT('',(2.1213203435595,-13.,-3.5));
#16805=CARTESIAN_POINT('',(-2.828427124746,-13.,3.5));
#16806=CARTESIAN_POINT('Origin',(0.,-13.,0.));
#16807=CARTESIAN_POINT('',(-3.162277660168,-13.,3.5));
#16808=CARTESIAN_POINT('',(-2.1213203435595,-13.,3.5));
#16809=CARTESIAN_POINT('',(-4.969293465979,-13.,2.357142857143));
#16810=CARTESIAN_POINT('Origin',(-3.162277660168,-13.,1.5));
#16811=CARTESIAN_POINT('Origin',(0.,-13.,0.));
#16812=CARTESIAN_POINT('Origin',(0.,-13.,0.));
#16813=CARTESIAN_POINT('',(-2.14313189850787E-16,-19.,1.75));
#16814=CARTESIAN_POINT('',(-2.14313189850787E-16,-13.,1.75));
#16815=CARTESIAN_POINT('Origin',(0.,-19.,0.));
#16816=CARTESIAN_POINT('Origin',(0.,-19.,0.));
#16817=CARTESIAN_POINT('',(-4.28626379701574E-16,-19.,3.5));
#16818=CARTESIAN_POINT('Origin',(0.,-19.,0.));
#16819=CARTESIAN_POINT('Origin',(0.,-13.,0.));
#16820=CARTESIAN_POINT('',(0.,-14.,3.5));
#16821=CARTESIAN_POINT('',(-4.28626379701574E-16,-13.,3.5));
#16822=CARTESIAN_POINT('',(0.,-14.,-3.5));
#16823=CARTESIAN_POINT('Origin',(0.,-14.,0.));
#16824=CARTESIAN_POINT('Origin',(0.,-14.,0.));
#16825=CARTESIAN_POINT('Origin',(0.,-14.,0.));
#16826=CARTESIAN_POINT('Ctrl Pts',(2.82842712474619,-13.,3.5));
#16827=CARTESIAN_POINT('Ctrl Pts',(1.86608944987721,-13.0000000000001,3.5));
#16828=CARTESIAN_POINT('Ctrl Pts',(0.848702054990486,-13.5463496695392,
3.5));
#16829=CARTESIAN_POINT('Ctrl Pts',(0.,-14.,3.5));
#16830=CARTESIAN_POINT('Ctrl Pts',(0.,-14.,-3.5));
#16831=CARTESIAN_POINT('Ctrl Pts',(0.848702054990486,-13.5463496695392,
-3.5));
#16832=CARTESIAN_POINT('Ctrl Pts',(1.86608944987721,-13.,-3.5));
#16833=CARTESIAN_POINT('Ctrl Pts',(2.82842712474619,-13.,-3.5));
#16834=CARTESIAN_POINT('Origin',(4.242640687119,0.,-3.5));
#16835=CARTESIAN_POINT('',(3.162277660168,0.,-3.5));
#16836=CARTESIAN_POINT('Ctrl Pts',(-2.82842712474619,-13.,-3.5));
#16837=CARTESIAN_POINT('Ctrl Pts',(-1.86608944987721,-13.0000000000001,
-3.5));
#16838=CARTESIAN_POINT('Ctrl Pts',(-0.848702054990486,-13.5463496695392,
-3.5));
#16839=CARTESIAN_POINT('Ctrl Pts',(0.,-14.,-3.5));
#16840=CARTESIAN_POINT('',(-3.162277660168,0.,-3.5));
#16841=CARTESIAN_POINT('',(-2.44929359829471E-16,-3.,-3.5));
#16842=CARTESIAN_POINT('Origin',(0.,-5.,-3.5));
#16843=CARTESIAN_POINT('Origin',(0.,-5.,-4.8));
#16844=CARTESIAN_POINT('',(-2.44929359829471E-16,-3.,3.5));
#16845=CARTESIAN_POINT('',(-2.44929359829471E-16,-3.,-4.8));
#16846=CARTESIAN_POINT('Origin',(0.,-5.,3.5));
#16847=CARTESIAN_POINT('Origin',(-4.242640687119,0.,3.5));
#16848=CARTESIAN_POINT('',(-3.162277660168,0.,3.5));
#16849=CARTESIAN_POINT('Ctrl Pts',(0.,-14.,3.5));
#16850=CARTESIAN_POINT('Ctrl Pts',(-0.848702054990486,-13.5463496695392,
3.5));
#16851=CARTESIAN_POINT('Ctrl Pts',(-1.86608944987721,-13.,3.5));
#16852=CARTESIAN_POINT('Ctrl Pts',(-2.82842712474619,-13.,3.5));
#16853=CARTESIAN_POINT('Origin',(0.,-14.,0.));
#16854=CARTESIAN_POINT('Origin',(-3.162277660168,24.7684,1.5));
#16855=CARTESIAN_POINT('',(-4.969293465979,0.,2.357142857143));
#16856=CARTESIAN_POINT('Origin',(0.,0.,0.));
#16857=CARTESIAN_POINT('',(-4.969293465979,0.,-2.357142857143));
#16858=CARTESIAN_POINT('Origin',(-3.162277660168,24.7684,-1.5));
#16859=CARTESIAN_POINT('Origin',(3.162277660168,24.7684,-1.5));
#16860=CARTESIAN_POINT('',(4.969293465979,0.,-2.357142857143));
#16861=CARTESIAN_POINT('Origin',(0.,0.,0.));
#16862=CARTESIAN_POINT('Origin',(0.,-19.,0.));
#16863=CARTESIAN_POINT('',(-2.,-19.,-2.44929359829471E-16));
#16864=CARTESIAN_POINT('Origin',(0.,-19.,0.));
#16865=CARTESIAN_POINT('',(-2.,-13.,-2.44929359829471E-16));
#16866=CARTESIAN_POINT('',(-2.,-19.,-2.44929359829471E-16));
#16867=CARTESIAN_POINT('Origin',(0.,-13.,0.));
#16868=CARTESIAN_POINT('Origin',(0.,-13.,0.));
#16869=CARTESIAN_POINT('',(1.75,-13.,0.));
#16870=CARTESIAN_POINT('Origin',(0.,-13.,0.));
#16871=CARTESIAN_POINT('',(0.,0.,0.));
#16872=CARTESIAN_POINT('Origin',(0.,0.,0.));
#16873=CARTESIAN_POINT('',(-2.,0.,2.44929359829471E-16));
#16874=CARTESIAN_POINT('Origin',(0.,0.,0.));
#16875=CARTESIAN_POINT('',(-1.83697019872103E-16,0.,1.5));
#16876=CARTESIAN_POINT('Origin',(0.,0.,0.));
#16877=CARTESIAN_POINT('Origin',(0.,0.,0.));
#16878=CARTESIAN_POINT('',(-2.,59.,2.44929359829471E-16));
#16879=CARTESIAN_POINT('Origin',(0.,59.,0.));
#16880=CARTESIAN_POINT('',(-2.,0.,2.44929359829471E-16));
#16881=CARTESIAN_POINT('Origin',(0.,59.,0.));
#16882=CARTESIAN_POINT('Origin',(0.,0.,0.));
#16883=CARTESIAN_POINT('',(-1.83697019872103E-16,-8.,1.5));
#16884=CARTESIAN_POINT('Origin',(0.,-8.,0.));
#16885=CARTESIAN_POINT('',(-1.83697019872103E-16,0.,1.5));
#16886=CARTESIAN_POINT('Origin',(0.,-8.,0.));
#16887=CARTESIAN_POINT('Origin',(0.,-8.,0.));
#16888=CARTESIAN_POINT('',(-1.25,-8.,-1.53080849893419E-16));
#16889=CARTESIAN_POINT('Origin',(0.,-8.,0.));
#16890=CARTESIAN_POINT('',(-1.25,0.,-1.53080849893419E-16));
#16891=CARTESIAN_POINT('',(-1.25,-8.,-1.53080849893419E-16));
#16892=CARTESIAN_POINT('Origin',(0.,0.,0.));
#16893=CARTESIAN_POINT('Origin',(0.,0.,0.));
#16894=CARTESIAN_POINT('',(1.5,0.,0.));
#16895=CARTESIAN_POINT('Origin',(0.,0.,0.));
#16896=CARTESIAN_POINT('Origin',(0.,59.,0.));
#16897=CARTESIAN_POINT('',(1.75,59.,-2.14313189850787E-16));
#16898=CARTESIAN_POINT('Origin',(0.,59.,0.));
#16899=CARTESIAN_POINT('',(1.75,52.,-2.14313189850787E-16));
#16900=CARTESIAN_POINT('',(1.75,59.,-2.14313189850787E-16));
#16901=CARTESIAN_POINT('Origin',(0.,52.,0.));
#16902=CARTESIAN_POINT('Origin',(0.,52.,0.));
#16903=CARTESIAN_POINT('',(-2.,52.,0.));
#16904=CARTESIAN_POINT('Origin',(0.,52.,0.));
#16905=CARTESIAN_POINT('',(0.,0.,0.));
#16906=CARTESIAN_POINT('Origin',(0.,0.,0.));
#16907=CARTESIAN_POINT('',(0.,8.,0.));
#16908=CARTESIAN_POINT('Origin',(0.,0.,0.));
#16909=CARTESIAN_POINT('',(0.,1.25,0.));
#16910=CARTESIAN_POINT('Origin',(0.,0.,0.));
#16911=CARTESIAN_POINT('Origin',(0.,0.,0.4));
#16912=CARTESIAN_POINT('',(0.,1.25,-8.));
#16913=CARTESIAN_POINT('',(1.53080849893419E-16,1.25,0.4));
#16914=CARTESIAN_POINT('Origin',(0.,0.,-8.));
#16915=CARTESIAN_POINT('Origin',(0.,0.,-8.));
#16916=CARTESIAN_POINT('',(0.,8.,-8.));
#16917=CARTESIAN_POINT('Origin',(0.,0.,-8.));
#16918=CARTESIAN_POINT('Origin',(0.,0.,0.4));
#16919=CARTESIAN_POINT('',(0.,8.,-4.75));
#16920=CARTESIAN_POINT('',(9.79717439317883E-16,8.,0.4));
#16921=CARTESIAN_POINT('Origin',(0.,0.,-4.75));
#16922=CARTESIAN_POINT('Origin',(0.,0.,-4.75));
#16923=CARTESIAN_POINT('',(0.,6.75,-4.75));
#16924=CARTESIAN_POINT('Origin',(0.,0.,-4.75));
#16925=CARTESIAN_POINT('Origin',(0.,0.,0.4));
#16926=CARTESIAN_POINT('',(0.,6.75,-3.25));
#16927=CARTESIAN_POINT('',(8.26636589424463E-16,6.75,0.4));
#16928=CARTESIAN_POINT('Origin',(0.,0.,-3.25));
#16929=CARTESIAN_POINT('Origin',(0.,0.,-3.25));
#16930=CARTESIAN_POINT('',(0.,8.,-3.25));
#16931=CARTESIAN_POINT('Origin',(0.,0.,-3.25));
#16932=CARTESIAN_POINT('Origin',(0.,0.,0.4));
#16933=CARTESIAN_POINT('',(9.79717439317883E-16,8.,0.4));
#16934=CARTESIAN_POINT('Origin',(0.,0.,-8.));
#16935=CARTESIAN_POINT('',(1.5,-1.83697019872103E-16,-8.));
#16936=CARTESIAN_POINT('Origin',(0.,0.,-8.));
#16937=CARTESIAN_POINT('',(1.5,-1.83697019872103E-16,0.));
#16938=CARTESIAN_POINT('',(1.5,-1.83697019872103E-16,-8.));
#16939=CARTESIAN_POINT('Origin',(0.,0.,0.));
#16940=CARTESIAN_POINT('Origin',(0.,0.,0.));
#16941=CARTESIAN_POINT('',(-1.25,0.,0.));
#16942=CARTESIAN_POINT('Origin',(0.,0.,0.));
#16943=CARTESIAN_POINT('',(0.,0.,0.));
#16944=CARTESIAN_POINT('',(0.,-72.,0.));
#16945=CARTESIAN_POINT('',(0.,-72.,0.));
#16946=CARTESIAN_POINT('',(0.,0.,0.));
#16947=CARTESIAN_POINT('',(0.,0.,-55.));
#16948=CARTESIAN_POINT('',(37.,0.,-22.));
#16949=CARTESIAN_POINT('',(44.,0.,-22.));
#16950=CARTESIAN_POINT('',(0.,0.,-96.93));
#16951=CARTESIAN_POINT('',(0.,0.,0.));
#16952=CARTESIAN_POINT('Origin',(0.,0.,-0.5));
#16953=CARTESIAN_POINT('',(-29.,5.,-0.5));
#16954=CARTESIAN_POINT('',(-31.,3.,-0.5));
#16955=CARTESIAN_POINT('Origin',(-29.,3.,-0.5));
#16956=CARTESIAN_POINT('',(29.,5.,-0.5));
#16957=CARTESIAN_POINT('',(29.,5.,-0.5));
#16958=CARTESIAN_POINT('',(31.,3.,-0.5));
#16959=CARTESIAN_POINT('Origin',(29.,3.,-0.5));
#16960=CARTESIAN_POINT('',(31.,-3.,-0.5));
#16961=CARTESIAN_POINT('',(31.,-3.,-0.5));
#16962=CARTESIAN_POINT('',(29.,-5.,-0.5));
#16963=CARTESIAN_POINT('Origin',(29.,-3.,-0.5));
#16964=CARTESIAN_POINT('',(-29.,-5.,-0.5));
#16965=CARTESIAN_POINT('',(-29.,-5.,-0.5));
#16966=CARTESIAN_POINT('',(-31.,-3.,-0.5));
#16967=CARTESIAN_POINT('Origin',(-29.,-3.,-0.5));
#16968=CARTESIAN_POINT('',(-31.,3.,-0.5));
#16969=CARTESIAN_POINT('',(24.5,0.,-0.5));
#16970=CARTESIAN_POINT('Origin',(26.,0.,-0.5));
#16971=CARTESIAN_POINT('',(-27.5,0.,-0.5));
#16972=CARTESIAN_POINT('Origin',(-26.,0.,-0.5));
#16973=CARTESIAN_POINT('Origin',(-26.,0.,-0.5));
#16974=CARTESIAN_POINT('',(-27.5,0.,0.));
#16975=CARTESIAN_POINT('',(-27.5,-1.83697019872103E-16,-0.5));
#16976=CARTESIAN_POINT('Origin',(-26.,0.,0.));
#16977=CARTESIAN_POINT('Origin',(0.,0.,0.));
#16978=CARTESIAN_POINT('',(-29.,4.,0.));
#16979=CARTESIAN_POINT('',(-30.,3.,0.));
#16980=CARTESIAN_POINT('Origin',(-29.,3.,0.));
#16981=CARTESIAN_POINT('',(-30.,-3.,0.));
#16982=CARTESIAN_POINT('',(-30.,3.,0.));
#16983=CARTESIAN_POINT('',(-29.,-4.,0.));
#16984=CARTESIAN_POINT('Origin',(-29.,-3.,0.));
#16985=CARTESIAN_POINT('',(29.,-4.,0.));
#16986=CARTESIAN_POINT('',(-29.,-4.,0.));
#16987=CARTESIAN_POINT('',(30.,-3.,0.));
#16988=CARTESIAN_POINT('Origin',(29.,-3.,0.));
#16989=CARTESIAN_POINT('',(30.,3.,0.));
#16990=CARTESIAN_POINT('',(30.,-3.,0.));
#16991=CARTESIAN_POINT('',(29.,4.,0.));
#16992=CARTESIAN_POINT('Origin',(29.,3.,0.));
#16993=CARTESIAN_POINT('',(29.,4.,0.));
#16994=CARTESIAN_POINT('',(24.5,0.,0.));
#16995=CARTESIAN_POINT('Origin',(26.,0.,0.));
#16996=CARTESIAN_POINT('Origin',(-29.,3.,0.5));
#16997=CARTESIAN_POINT('',(-29.,4.,0.5));
#16998=CARTESIAN_POINT('',(-30.,3.,0.5));
#16999=CARTESIAN_POINT('Origin',(-29.,3.,0.5));
#17000=CARTESIAN_POINT('',(-30.,3.,0.5));
#17001=CARTESIAN_POINT('',(-29.,4.,0.5));
#17002=CARTESIAN_POINT('Origin',(0.,0.,0.5));
#17003=CARTESIAN_POINT('',(-29.,5.,0.5));
#17004=CARTESIAN_POINT('',(-31.,3.,0.5));
#17005=CARTESIAN_POINT('Origin',(-29.,3.,0.5));
#17006=CARTESIAN_POINT('',(-31.,-3.,0.5));
#17007=CARTESIAN_POINT('',(-31.,3.,0.5));
#17008=CARTESIAN_POINT('',(-29.,-5.,0.5));
#17009=CARTESIAN_POINT('Origin',(-29.,-3.,0.5));
#17010=CARTESIAN_POINT('',(29.,-5.,0.5));
#17011=CARTESIAN_POINT('',(-29.,-5.,0.5));
#17012=CARTESIAN_POINT('',(31.,-3.,0.5));
#17013=CARTESIAN_POINT('Origin',(29.,-3.,0.5));
#17014=CARTESIAN_POINT('',(31.,3.,0.5));
#17015=CARTESIAN_POINT('',(31.,-3.,0.5));
#17016=CARTESIAN_POINT('',(29.,5.,0.5));
#17017=CARTESIAN_POINT('Origin',(29.,3.,0.5));
#17018=CARTESIAN_POINT('',(29.,5.,0.5));
#17019=CARTESIAN_POINT('',(29.,4.,0.5));
#17020=CARTESIAN_POINT('',(29.,4.,0.5));
#17021=CARTESIAN_POINT('',(30.,3.,0.5));
#17022=CARTESIAN_POINT('Origin',(29.,3.,0.5));
#17023=CARTESIAN_POINT('',(30.,-3.,0.5));
#17024=CARTESIAN_POINT('',(30.,-3.,0.5));
#17025=CARTESIAN_POINT('',(29.,-4.,0.5));
#17026=CARTESIAN_POINT('Origin',(29.,-3.,0.5));
#17027=CARTESIAN_POINT('',(-29.,-4.,0.5));
#17028=CARTESIAN_POINT('',(-29.,-4.,0.5));
#17029=CARTESIAN_POINT('',(-30.,-3.,0.5));
#17030=CARTESIAN_POINT('Origin',(-29.,-3.,0.5));
#17031=CARTESIAN_POINT('',(-30.,3.,0.5));
#17032=CARTESIAN_POINT('Origin',(-29.,3.,-0.5));
#17033=CARTESIAN_POINT('',(-31.,3.,-0.5));
#17034=CARTESIAN_POINT('',(-29.,5.,-0.5));
#17035=CARTESIAN_POINT('Origin',(29.,5.,-0.5));
#17036=CARTESIAN_POINT('',(29.,5.,-0.5));
#17037=CARTESIAN_POINT('Origin',(29.,3.,-0.5));
#17038=CARTESIAN_POINT('',(31.,3.,-0.5));
#17039=CARTESIAN_POINT('Origin',(31.,-3.,-0.5));
#17040=CARTESIAN_POINT('',(31.,-3.,-0.5));
#17041=CARTESIAN_POINT('Origin',(29.,-3.,-0.5));
#17042=CARTESIAN_POINT('',(29.,-5.,-0.5));
#17043=CARTESIAN_POINT('Origin',(-29.,-5.,-0.5));
#17044=CARTESIAN_POINT('',(-29.,-5.,-0.5));
#17045=CARTESIAN_POINT('Origin',(-29.,-3.,-0.5));
#17046=CARTESIAN_POINT('',(-31.,-3.,-0.5));
#17047=CARTESIAN_POINT('Origin',(-31.,3.,-0.5));
#17048=CARTESIAN_POINT('Origin',(-30.,3.,0.5));
#17049=CARTESIAN_POINT('',(-30.,-3.,0.5));
#17050=CARTESIAN_POINT('Origin',(-29.,-3.,0.5));
#17051=CARTESIAN_POINT('',(-29.,-4.,0.5));
#17052=CARTESIAN_POINT('Origin',(-29.,-4.,0.5));
#17053=CARTESIAN_POINT('',(29.,-4.,0.5));
#17054=CARTESIAN_POINT('Origin',(29.,-3.,0.5));
#17055=CARTESIAN_POINT('',(30.,-3.,0.5));
#17056=CARTESIAN_POINT('Origin',(30.,-3.,0.5));
#17057=CARTESIAN_POINT('',(30.,3.,0.5));
#17058=CARTESIAN_POINT('Origin',(29.,3.,0.5));
#17059=CARTESIAN_POINT('',(29.,4.,0.5));
#17060=CARTESIAN_POINT('Origin',(29.,4.,0.5));
#17061=CARTESIAN_POINT('Origin',(26.,0.,-0.5));
#17062=CARTESIAN_POINT('',(24.5,-1.83697019872103E-16,-0.5));
#17063=CARTESIAN_POINT('',(0.,0.,0.));
#17064=CARTESIAN_POINT('',(0.,25.,0.));
#17065=CARTESIAN_POINT('',(0.,140.,-17.5));
#17066=CARTESIAN_POINT('',(-4.481237553453,39.4612323939,22.));
#17067=CARTESIAN_POINT('',(-3.198173628563E-5,14.38936550283,54.57904729942));
#17068=UNCERTAINTY_MEASURE_WITH_UNIT(LENGTH_MEASURE(0.01),#17114,
'DISTANCE_ACCURACY_VALUE',
'Maximum model space distance between geometric entities at asserted c
onnectivities');
#17069=UNCERTAINTY_MEASURE_WITH_UNIT(LENGTH_MEASURE(0.01),#17114,
'DISTANCE_ACCURACY_VALUE',
'Maximum model space distance between geometric entities at asserted c
onnectivities');
#17070=UNCERTAINTY_MEASURE_WITH_UNIT(LENGTH_MEASURE(0.01),#17114,
'DISTANCE_ACCURACY_VALUE',
'Maximum model space distance between geometric entities at asserted c
onnectivities');
#17071=UNCERTAINTY_MEASURE_WITH_UNIT(LENGTH_MEASURE(0.01),#17114,
'DISTANCE_ACCURACY_VALUE',
'Maximum model space distance between geometric entities at asserted c
onnectivities');
#17072=UNCERTAINTY_MEASURE_WITH_UNIT(LENGTH_MEASURE(0.01),#17114,
'DISTANCE_ACCURACY_VALUE',
'Maximum model space distance between geometric entities at asserted c
onnectivities');
#17073=UNCERTAINTY_MEASURE_WITH_UNIT(LENGTH_MEASURE(0.01),#17114,
'DISTANCE_ACCURACY_VALUE',
'Maximum model space distance between geometric entities at asserted c
onnectivities');
#17074=UNCERTAINTY_MEASURE_WITH_UNIT(LENGTH_MEASURE(0.01),#17114,
'DISTANCE_ACCURACY_VALUE',
'Maximum model space distance between geometric entities at asserted c
onnectivities');
#17075=UNCERTAINTY_MEASURE_WITH_UNIT(LENGTH_MEASURE(0.01),#17114,
'DISTANCE_ACCURACY_VALUE',
'Maximum model space distance between geometric entities at asserted c
onnectivities');
#17076=UNCERTAINTY_MEASURE_WITH_UNIT(LENGTH_MEASURE(0.01),#17114,
'DISTANCE_ACCURACY_VALUE',
'Maximum model space distance between geometric entities at asserted c
onnectivities');
#17077=UNCERTAINTY_MEASURE_WITH_UNIT(LENGTH_MEASURE(0.01),#17114,
'DISTANCE_ACCURACY_VALUE',
'Maximum model space distance between geometric entities at asserted c
onnectivities');
#17078=UNCERTAINTY_MEASURE_WITH_UNIT(LENGTH_MEASURE(0.01),#17114,
'DISTANCE_ACCURACY_VALUE',
'Maximum model space distance between geometric entities at asserted c
onnectivities');
#17079=UNCERTAINTY_MEASURE_WITH_UNIT(LENGTH_MEASURE(0.01),#17114,
'DISTANCE_ACCURACY_VALUE',
'Maximum model space distance between geometric entities at asserted c
onnectivities');
#17080=UNCERTAINTY_MEASURE_WITH_UNIT(LENGTH_MEASURE(0.01),#17114,
'DISTANCE_ACCURACY_VALUE',
'Maximum model space distance between geometric entities at asserted c
onnectivities');
#17081=UNCERTAINTY_MEASURE_WITH_UNIT(LENGTH_MEASURE(0.01),#17114,
'DISTANCE_ACCURACY_VALUE',
'Maximum model space distance between geometric entities at asserted c
onnectivities');
#17082=UNCERTAINTY_MEASURE_WITH_UNIT(LENGTH_MEASURE(0.01),#17114,
'DISTANCE_ACCURACY_VALUE',
'Maximum model space distance between geometric entities at asserted c
onnectivities');
#17083=UNCERTAINTY_MEASURE_WITH_UNIT(LENGTH_MEASURE(0.01),#17114,
'DISTANCE_ACCURACY_VALUE',
'Maximum model space distance between geometric entities at asserted c
onnectivities');
#17084=UNCERTAINTY_MEASURE_WITH_UNIT(LENGTH_MEASURE(0.01),#17114,
'DISTANCE_ACCURACY_VALUE',
'Maximum model space distance between geometric entities at asserted c
onnectivities');
#17085=UNCERTAINTY_MEASURE_WITH_UNIT(LENGTH_MEASURE(0.01),#17114,
'DISTANCE_ACCURACY_VALUE',
'Maximum model space distance between geometric entities at asserted c
onnectivities');
#17086=UNCERTAINTY_MEASURE_WITH_UNIT(LENGTH_MEASURE(0.01),#17114,
'DISTANCE_ACCURACY_VALUE',
'Maximum model space distance between geometric entities at asserted c
onnectivities');
#17087=UNCERTAINTY_MEASURE_WITH_UNIT(LENGTH_MEASURE(0.01),#17114,
'DISTANCE_ACCURACY_VALUE',
'Maximum model space distance between geometric entities at asserted c
onnectivities');
#17088=UNCERTAINTY_MEASURE_WITH_UNIT(LENGTH_MEASURE(0.01),#17114,
'DISTANCE_ACCURACY_VALUE',
'Maximum model space distance between geometric entities at asserted c
onnectivities');
#17089=UNCERTAINTY_MEASURE_WITH_UNIT(LENGTH_MEASURE(0.01),#17114,
'DISTANCE_ACCURACY_VALUE',
'Maximum model space distance between geometric entities at asserted c
onnectivities');
#17090=UNCERTAINTY_MEASURE_WITH_UNIT(LENGTH_MEASURE(0.01),#17114,
'DISTANCE_ACCURACY_VALUE',
'Maximum model space distance between geometric entities at asserted c
onnectivities');
#17091=(
GEOMETRIC_REPRESENTATION_CONTEXT(3)
GLOBAL_UNCERTAINTY_ASSIGNED_CONTEXT((#17068))
GLOBAL_UNIT_ASSIGNED_CONTEXT((#17114,#17116,#17117))
REPRESENTATION_CONTEXT('','3D')
);
#17092=(
GEOMETRIC_REPRESENTATION_CONTEXT(3)
GLOBAL_UNCERTAINTY_ASSIGNED_CONTEXT((#17069))
GLOBAL_UNIT_ASSIGNED_CONTEXT((#17114,#17116,#17117))
REPRESENTATION_CONTEXT('','3D')
);
#17093=(
GEOMETRIC_REPRESENTATION_CONTEXT(3)
GLOBAL_UNCERTAINTY_ASSIGNED_CONTEXT((#17070))
GLOBAL_UNIT_ASSIGNED_CONTEXT((#17114,#17116,#17117))
REPRESENTATION_CONTEXT('','3D')
);
#17094=(
GEOMETRIC_REPRESENTATION_CONTEXT(3)
GLOBAL_UNCERTAINTY_ASSIGNED_CONTEXT((#17071))
GLOBAL_UNIT_ASSIGNED_CONTEXT((#17114,#17116,#17117))
REPRESENTATION_CONTEXT('','3D')
);
#17095=(
GEOMETRIC_REPRESENTATION_CONTEXT(3)
GLOBAL_UNCERTAINTY_ASSIGNED_CONTEXT((#17072))
GLOBAL_UNIT_ASSIGNED_CONTEXT((#17114,#17116,#17117))
REPRESENTATION_CONTEXT('','3D')
);
#17096=(
GEOMETRIC_REPRESENTATION_CONTEXT(3)
GLOBAL_UNCERTAINTY_ASSIGNED_CONTEXT((#17073))
GLOBAL_UNIT_ASSIGNED_CONTEXT((#17114,#17116,#17117))
REPRESENTATION_CONTEXT('','3D')
);
#17097=(
GEOMETRIC_REPRESENTATION_CONTEXT(3)
GLOBAL_UNCERTAINTY_ASSIGNED_CONTEXT((#17074))
GLOBAL_UNIT_ASSIGNED_CONTEXT((#17114,#17116,#17117))
REPRESENTATION_CONTEXT('','3D')
);
#17098=(
GEOMETRIC_REPRESENTATION_CONTEXT(3)
GLOBAL_UNCERTAINTY_ASSIGNED_CONTEXT((#17075))
GLOBAL_UNIT_ASSIGNED_CONTEXT((#17114,#17116,#17117))
REPRESENTATION_CONTEXT('','3D')
);
#17099=(
GEOMETRIC_REPRESENTATION_CONTEXT(3)
GLOBAL_UNCERTAINTY_ASSIGNED_CONTEXT((#17076))
GLOBAL_UNIT_ASSIGNED_CONTEXT((#17114,#17116,#17117))
REPRESENTATION_CONTEXT('','3D')
);
#17100=(
GEOMETRIC_REPRESENTATION_CONTEXT(3)
GLOBAL_UNCERTAINTY_ASSIGNED_CONTEXT((#17077))
GLOBAL_UNIT_ASSIGNED_CONTEXT((#17114,#17116,#17117))
REPRESENTATION_CONTEXT('','3D')
);
#17101=(
GEOMETRIC_REPRESENTATION_CONTEXT(3)
GLOBAL_UNCERTAINTY_ASSIGNED_CONTEXT((#17078))
GLOBAL_UNIT_ASSIGNED_CONTEXT((#17114,#17116,#17117))
REPRESENTATION_CONTEXT('','3D')
);
#17102=(
GEOMETRIC_REPRESENTATION_CONTEXT(3)
GLOBAL_UNCERTAINTY_ASSIGNED_CONTEXT((#17079))
GLOBAL_UNIT_ASSIGNED_CONTEXT((#17114,#17116,#17117))
REPRESENTATION_CONTEXT('','3D')
);
#17103=(
GEOMETRIC_REPRESENTATION_CONTEXT(3)
GLOBAL_UNCERTAINTY_ASSIGNED_CONTEXT((#17080))
GLOBAL_UNIT_ASSIGNED_CONTEXT((#17114,#17116,#17117))
REPRESENTATION_CONTEXT('','3D')
);
#17104=(
GEOMETRIC_REPRESENTATION_CONTEXT(3)
GLOBAL_UNCERTAINTY_ASSIGNED_CONTEXT((#17081))
GLOBAL_UNIT_ASSIGNED_CONTEXT((#17114,#17116,#17117))
REPRESENTATION_CONTEXT('','3D')
);
#17105=(
GEOMETRIC_REPRESENTATION_CONTEXT(3)
GLOBAL_UNCERTAINTY_ASSIGNED_CONTEXT((#17082))
GLOBAL_UNIT_ASSIGNED_CONTEXT((#17114,#17116,#17117))
REPRESENTATION_CONTEXT('','3D')
);
#17106=(
GEOMETRIC_REPRESENTATION_CONTEXT(3)
GLOBAL_UNCERTAINTY_ASSIGNED_CONTEXT((#17083))
GLOBAL_UNIT_ASSIGNED_CONTEXT((#17114,#17116,#17117))
REPRESENTATION_CONTEXT('','3D')
);
#17107=(
GEOMETRIC_REPRESENTATION_CONTEXT(3)
GLOBAL_UNCERTAINTY_ASSIGNED_CONTEXT((#17084))
GLOBAL_UNIT_ASSIGNED_CONTEXT((#17114,#17116,#17117))
REPRESENTATION_CONTEXT('','3D')
);
#17108=(
GEOMETRIC_REPRESENTATION_CONTEXT(3)
GLOBAL_UNCERTAINTY_ASSIGNED_CONTEXT((#17085))
GLOBAL_UNIT_ASSIGNED_CONTEXT((#17114,#17116,#17117))
REPRESENTATION_CONTEXT('','3D')
);
#17109=(
GEOMETRIC_REPRESENTATION_CONTEXT(3)
GLOBAL_UNCERTAINTY_ASSIGNED_CONTEXT((#17086))
GLOBAL_UNIT_ASSIGNED_CONTEXT((#17114,#17116,#17117))
REPRESENTATION_CONTEXT('','3D')
);
#17110=(
GEOMETRIC_REPRESENTATION_CONTEXT(3)
GLOBAL_UNCERTAINTY_ASSIGNED_CONTEXT((#17087))
GLOBAL_UNIT_ASSIGNED_CONTEXT((#17114,#17116,#17117))
REPRESENTATION_CONTEXT('','3D')
);
#17111=(
GEOMETRIC_REPRESENTATION_CONTEXT(3)
GLOBAL_UNCERTAINTY_ASSIGNED_CONTEXT((#17088))
GLOBAL_UNIT_ASSIGNED_CONTEXT((#17114,#17116,#17117))
REPRESENTATION_CONTEXT('','3D')
);
#17112=(
GEOMETRIC_REPRESENTATION_CONTEXT(3)
GLOBAL_UNCERTAINTY_ASSIGNED_CONTEXT((#17089))
GLOBAL_UNIT_ASSIGNED_CONTEXT((#17114,#17116,#17117))
REPRESENTATION_CONTEXT('','3D')
);
#17113=(
GEOMETRIC_REPRESENTATION_CONTEXT(3)
GLOBAL_UNCERTAINTY_ASSIGNED_CONTEXT((#17090))
GLOBAL_UNIT_ASSIGNED_CONTEXT((#17114,#17116,#17117))
REPRESENTATION_CONTEXT('','3D')
);
#17114=(
LENGTH_UNIT()
NAMED_UNIT(*)
SI_UNIT(.MILLI.,.METRE.)
);
#17115=(
LENGTH_UNIT()
NAMED_UNIT(*)
SI_UNIT($,.METRE.)
);
#17116=(
NAMED_UNIT(*)
PLANE_ANGLE_UNIT()
SI_UNIT($,.RADIAN.)
);
#17117=(
NAMED_UNIT(*)
SI_UNIT($,.STERADIAN.)
SOLID_ANGLE_UNIT()
);
#17118=SHAPE_DEFINITION_REPRESENTATION(#17140,#17184);
#17119=SHAPE_DEFINITION_REPRESENTATION(#17141,#17185);
#17120=SHAPE_DEFINITION_REPRESENTATION(#17142,#17186);
#17121=SHAPE_DEFINITION_REPRESENTATION(#17143,#17187);
#17122=SHAPE_DEFINITION_REPRESENTATION(#17144,#17188);
#17123=SHAPE_DEFINITION_REPRESENTATION(#17145,#17189);
#17124=SHAPE_DEFINITION_REPRESENTATION(#17150,#17190);
#17125=SHAPE_DEFINITION_REPRESENTATION(#17151,#17191);
#17126=SHAPE_DEFINITION_REPRESENTATION(#17152,#17192);
#17127=SHAPE_DEFINITION_REPRESENTATION(#17153,#17193);
#17128=SHAPE_DEFINITION_REPRESENTATION(#17154,#17194);
#17129=SHAPE_DEFINITION_REPRESENTATION(#17155,#17195);
#17130=SHAPE_DEFINITION_REPRESENTATION(#17161,#17196);
#17131=SHAPE_DEFINITION_REPRESENTATION(#17162,#17197);
#17132=SHAPE_DEFINITION_REPRESENTATION(#17163,#17198);
#17133=SHAPE_DEFINITION_REPRESENTATION(#17164,#17199);
#17134=SHAPE_DEFINITION_REPRESENTATION(#17165,#17200);
#17135=SHAPE_DEFINITION_REPRESENTATION(#17166,#17201);
#17136=SHAPE_DEFINITION_REPRESENTATION(#17167,#17202);
#17137=SHAPE_DEFINITION_REPRESENTATION(#17168,#17203);
#17138=SHAPE_DEFINITION_REPRESENTATION(#17169,#17204);
#17139=SHAPE_DEFINITION_REPRESENTATION(#17178,#17205);
#17140=PRODUCT_DEFINITION_SHAPE('',$,#17207);
#17141=PRODUCT_DEFINITION_SHAPE('',$,#17208);
#17142=PRODUCT_DEFINITION_SHAPE('',$,#17209);
#17143=PRODUCT_DEFINITION_SHAPE('',$,#17210);
#17144=PRODUCT_DEFINITION_SHAPE('',$,#17211);
#17145=PRODUCT_DEFINITION_SHAPE('',$,#17212);
#17146=PRODUCT_DEFINITION_SHAPE($,$,#83);
#17147=PRODUCT_DEFINITION_SHAPE($,$,#84);
#17148=PRODUCT_DEFINITION_SHAPE($,$,#85);
#17149=PRODUCT_DEFINITION_SHAPE($,$,#86);
#17150=PRODUCT_DEFINITION_SHAPE('',$,#17213);
#17151=PRODUCT_DEFINITION_SHAPE('',$,#17214);
#17152=PRODUCT_DEFINITION_SHAPE('',$,#17215);
#17153=PRODUCT_DEFINITION_SHAPE('',$,#17216);
#17154=PRODUCT_DEFINITION_SHAPE('',$,#17217);
#17155=PRODUCT_DEFINITION_SHAPE('',$,#17218);
#17156=PRODUCT_DEFINITION_SHAPE($,$,#87);
#17157=PRODUCT_DEFINITION_SHAPE($,$,#88);
#17158=PRODUCT_DEFINITION_SHAPE($,$,#89);
#17159=PRODUCT_DEFINITION_SHAPE($,$,#90);
#17160=PRODUCT_DEFINITION_SHAPE($,$,#91);
#17161=PRODUCT_DEFINITION_SHAPE('',$,#17219);
#17162=PRODUCT_DEFINITION_SHAPE('',$,#17220);
#17163=PRODUCT_DEFINITION_SHAPE('',$,#17221);
#17164=PRODUCT_DEFINITION_SHAPE('',$,#17222);
#17165=PRODUCT_DEFINITION_SHAPE('',$,#17223);
#17166=PRODUCT_DEFINITION_SHAPE('',$,#17224);
#17167=PRODUCT_DEFINITION_SHAPE('',$,#17225);
#17168=PRODUCT_DEFINITION_SHAPE('',$,#17226);
#17169=PRODUCT_DEFINITION_SHAPE('',$,#17227);
#17170=PRODUCT_DEFINITION_SHAPE($,$,#92);
#17171=PRODUCT_DEFINITION_SHAPE($,$,#93);
#17172=PRODUCT_DEFINITION_SHAPE($,$,#94);
#17173=PRODUCT_DEFINITION_SHAPE($,$,#95);
#17174=PRODUCT_DEFINITION_SHAPE($,$,#96);
#17175=PRODUCT_DEFINITION_SHAPE($,$,#97);
#17176=PRODUCT_DEFINITION_SHAPE($,$,#98);
#17177=PRODUCT_DEFINITION_SHAPE($,$,#99);
#17178=PRODUCT_DEFINITION_SHAPE('',$,#17228);
#17179=PRODUCT_DEFINITION_SHAPE($,$,#100);
#17180=PRODUCT_DEFINITION_SHAPE($,$,#101);
#17181=PRODUCT_DEFINITION_SHAPE($,$,#102);
#17182=PRODUCT_DEFINITION_SHAPE($,$,#103);
#17183=PRODUCT_DEFINITION_SHAPE($,$,#104);
#17184=SHAPE_REPRESENTATION('',(#6209,#6973,#6974,#6975,#6976,#6977),#17091);
#17185=SHAPE_REPRESENTATION('',(#6210),#17092);
#17186=SHAPE_REPRESENTATION('',(#6241,#6553,#6554,#6555,#6556),#17093);
#17187=SHAPE_REPRESENTATION('',(#6242,#239,#240),#17094);
#17188=SHAPE_REPRESENTATION('',(#6301,#241,#242),#17095);
#17189=SHAPE_REPRESENTATION('',(#6523,#243,#244),#17096);
#17190=SHAPE_REPRESENTATION('',(#6557,#6700,#6701),#17097);
#17191=SHAPE_REPRESENTATION('',(#6558),#17098);
#17192=SHAPE_REPRESENTATION('',(#6609,#6697,#6698,#6699),#17099);
#17193=SHAPE_REPRESENTATION('',(#6610,#245),#17100);
#17194=SHAPE_REPRESENTATION('',(#6652,#246),#17101);
#17195=SHAPE_REPRESENTATION('',(#6679),#17102);
#17196=SHAPE_REPRESENTATION('',(#6702,#6926,#6927,#6928,#6929,#6930),#17103);
#17197=SHAPE_REPRESENTATION('',(#6703,#247,#248,#249,#250,#251),#17104);
#17198=SHAPE_REPRESENTATION('',(#6781),#17105);
#17199=SHAPE_REPRESENTATION('',(#6815),#17106);
#17200=SHAPE_REPRESENTATION('',(#6818,#252),#17107);
#17201=SHAPE_REPRESENTATION('',(#6835,#6923,#6924,#6925),#17108);
#17202=SHAPE_REPRESENTATION('',(#6836,#253),#17109);
#17203=SHAPE_REPRESENTATION('',(#6881,#254,#255),#17110);
#17204=SHAPE_REPRESENTATION('',(#6901,#256),#17111);
#17205=SHAPE_REPRESENTATION('',(#6931),#17112);
#17206=PRODUCT_DEFINITION_CONTEXT('part definition',#17274,'design');
#17207=PRODUCT_DEFINITION('STEAMENGINE_ASM',
'MAS-613',#17229,#17206);
#17208=PRODUCT_DEFINITION('base','BASE',#17230,#17206);
#17209=PRODUCT_DEFINITION('1_ASM','1_ASM',#17231,#17206);
#17210=PRODUCT_DEFINITION('BASEPLATE','BASEPLATE',#17232,#17206);
#17211=PRODUCT_DEFINITION('COLUMN','COLUMN',#17233,#17206);
#17212=PRODUCT_DEFINITION('IN-OUTLET','IN-OUTLET',#17234,#17206);
#17213=PRODUCT_DEFINITION('3_ASM','3_ASM',#17235,#17206);
#17214=PRODUCT_DEFINITION('FLYWHEEL','FLYWHEEL',#17236,#17206);
#17215=PRODUCT_DEFINITION('CRANKSHAFT_ASM','CRANKSHAFT_ASM',#17237,#17206);
#17216=PRODUCT_DEFINITION('7-2','7-2',#17238,#17206);
#17217=PRODUCT_DEFINITION('7-1','7-1',#17239,#17206);
#17218=PRODUCT_DEFINITION('7-3','7-3',#17240,#17206);
#17219=PRODUCT_DEFINITION('2_ASM','2_ASM',#17241,#17206);
#17220=PRODUCT_DEFINITION('Cylinder','CYLINDER',#17242,#17206);
#17221=PRODUCT_DEFINITION('CYLINDERCOVER','CYLINDERCOVER',#17243,#17206);
#17222=PRODUCT_DEFINITION('PRESSURESPRING','PRESSURESPRING',#17244,#17206);
#17223=PRODUCT_DEFINITION('Nut','NUT',#17245,#17206);
#17224=PRODUCT_DEFINITION('PISTON_ASM','PISTON_ASM',#17246,#17206);
#17225=PRODUCT_DEFINITION('6-1','6-1',#17247,#17206);
#17226=PRODUCT_DEFINITION('6-2','6-2',#17248,#17206);
#17227=PRODUCT_DEFINITION('6-3','6-3',#17249,#17206);
#17228=PRODUCT_DEFINITION('NAMEPLATE','NAMEPLATE',#17250,#17206);
#17229=PRODUCT_DEFINITION_FORMATION('',$,#17276);
#17230=PRODUCT_DEFINITION_FORMATION('',$,#17277);
#17231=PRODUCT_DEFINITION_FORMATION('',$,#17278);
#17232=PRODUCT_DEFINITION_FORMATION('',$,#17279);
#17233=PRODUCT_DEFINITION_FORMATION('',$,#17280);
#17234=PRODUCT_DEFINITION_FORMATION('',$,#17281);
#17235=PRODUCT_DEFINITION_FORMATION('',$,#17282);
#17236=PRODUCT_DEFINITION_FORMATION('',$,#17283);
#17237=PRODUCT_DEFINITION_FORMATION('',$,#17284);
#17238=PRODUCT_DEFINITION_FORMATION('',$,#17285);
#17239=PRODUCT_DEFINITION_FORMATION('',$,#17286);
#17240=PRODUCT_DEFINITION_FORMATION('',$,#17287);
#17241=PRODUCT_DEFINITION_FORMATION('',$,#17288);
#17242=PRODUCT_DEFINITION_FORMATION('',$,#17289);
#17243=PRODUCT_DEFINITION_FORMATION('',$,#17290);
#17244=PRODUCT_DEFINITION_FORMATION('',$,#17291);
#17245=PRODUCT_DEFINITION_FORMATION('',$,#17292);
#17246=PRODUCT_DEFINITION_FORMATION('',$,#17293);
#17247=PRODUCT_DEFINITION_FORMATION('',$,#17294);
#17248=PRODUCT_DEFINITION_FORMATION('',$,#17295);
#17249=PRODUCT_DEFINITION_FORMATION('',$,#17296);
#17250=PRODUCT_DEFINITION_FORMATION('',$,#17297);
#17251=PRODUCT_RELATED_PRODUCT_CATEGORY('MAS-613',
'MAS-613',(#17276));
#17252=PRODUCT_RELATED_PRODUCT_CATEGORY('BASE','BASE',(#17277));
#17253=PRODUCT_RELATED_PRODUCT_CATEGORY('1_ASM','1_ASM',(#17278));
#17254=PRODUCT_RELATED_PRODUCT_CATEGORY('BASEPLATE','BASEPLATE',(#17279));
#17255=PRODUCT_RELATED_PRODUCT_CATEGORY('COLUMN','COLUMN',(#17280));
#17256=PRODUCT_RELATED_PRODUCT_CATEGORY('IN-OUTLET','IN-OUTLET',(#17281));
#17257=PRODUCT_RELATED_PRODUCT_CATEGORY('3_ASM','3_ASM',(#17282));
#17258=PRODUCT_RELATED_PRODUCT_CATEGORY('FLYWHEEL','FLYWHEEL',(#17283));
#17259=PRODUCT_RELATED_PRODUCT_CATEGORY('CRANKSHAFT_ASM',
'CRANKSHAFT_ASM',(#17284));
#17260=PRODUCT_RELATED_PRODUCT_CATEGORY('7-2','7-2',(#17285));
#17261=PRODUCT_RELATED_PRODUCT_CATEGORY('7-1','7-1',(#17286));
#17262=PRODUCT_RELATED_PRODUCT_CATEGORY('7-3','7-3',(#17287));
#17263=PRODUCT_RELATED_PRODUCT_CATEGORY('2_ASM','2_ASM',(#17288));
#17264=PRODUCT_RELATED_PRODUCT_CATEGORY('CYLINDER','CYLINDER',(#17289));
#17265=PRODUCT_RELATED_PRODUCT_CATEGORY('CYLINDERCOVER','CYLINDERCOVER',
(#17290));
#17266=PRODUCT_RELATED_PRODUCT_CATEGORY('PRESSURESPRING',
'PRESSURESPRING',(#17291));
#17267=PRODUCT_RELATED_PRODUCT_CATEGORY('NUT','NUT',(#17292));
#17268=PRODUCT_RELATED_PRODUCT_CATEGORY('PISTON_ASM','PISTON_ASM',(#17293));
#17269=PRODUCT_RELATED_PRODUCT_CATEGORY('6-1','6-1',(#17294));
#17270=PRODUCT_RELATED_PRODUCT_CATEGORY('6-2','6-2',(#17295));
#17271=PRODUCT_RELATED_PRODUCT_CATEGORY('6-3','6-3',(#17296));
#17272=PRODUCT_RELATED_PRODUCT_CATEGORY('NAMEPLATE','NAMEPLATE',(#17297));
#17273=APPLICATION_PROTOCOL_DEFINITION('international standard',
'automotive_design',2009,#17274);
#17274=APPLICATION_CONTEXT(
'Core Data for Automotive Mechanical Design Process');
#17275=PRODUCT_CONTEXT('part definition',#17274,'mechanical');
#17276=PRODUCT('STEAMENGINE_ASM','MAS-613',$,(#17275));
#17277=PRODUCT('base','BASE',$,(#17275));
#17278=PRODUCT('1_ASM','1_ASM','NOT SPECIFIED',(#17275));
#17279=PRODUCT('BASEPLATE','BASEPLATE','NOT SPECIFIED',(#17275));
#17280=PRODUCT('COLUMN','COLUMN','NOT SPECIFIED',(#17275));
#17281=PRODUCT('IN-OUTLET','IN-OUTLET','NOT SPECIFIED',(#17275));
#17282=PRODUCT('3_ASM','3_ASM','NOT SPECIFIED',(#17275));
#17283=PRODUCT('FLYWHEEL','FLYWHEEL','NOT SPECIFIED',(#17275));
#17284=PRODUCT('CRANKSHAFT_ASM','CRANKSHAFT_ASM','NOT SPECIFIED',(#17275));
#17285=PRODUCT('7-2','7-2','NOT SPECIFIED',(#17275));
#17286=PRODUCT('7-1','7-1','NOT SPECIFIED',(#17275));
#17287=PRODUCT('7-3','7-3','NOT SPECIFIED',(#17275));
#17288=PRODUCT('2_ASM','2_ASM','NOT SPECIFIED',(#17275));
#17289=PRODUCT('Cylinder','CYLINDER',$,(#17275));
#17290=PRODUCT('CYLINDERCOVER','CYLINDERCOVER','NOT SPECIFIED',(#17275));
#17291=PRODUCT('PRESSURESPRING','PRESSURESPRING','NOT SPECIFIED',(#17275));
#17292=PRODUCT('Nut','NUT',$,(#17275));
#17293=PRODUCT('PISTON_ASM','PISTON_ASM','NOT SPECIFIED',(#17275));
#17294=PRODUCT('6-1','6-1','NOT SPECIFIED',(#17275));
#17295=PRODUCT('6-2','6-2','NOT SPECIFIED',(#17275));
#17296=PRODUCT('6-3','6-3','NOT SPECIFIED',(#17275));
#17297=PRODUCT('NAMEPLATE','NAMEPLATE','NOT SPECIFIED',(#17275));
#17298=PRESENTATION_STYLE_ASSIGNMENT((#17299));
#17299=SURFACE_STYLE_USAGE(.BOTH.,#17300);
#17300=SURFACE_SIDE_STYLE('',(#17301));
#17301=SURFACE_STYLE_FILL_AREA(#17302);
#17302=FILL_AREA_STYLE('Steel - Satin',(#17303));
#17303=FILL_AREA_STYLE_COLOUR('Steel - Satin',#17304);
#17304=COLOUR_RGB('Steel - Satin', 0.09019608, 0.27058824, 0.51372549);
ENDSEC;
END-ISO-10303-21;
